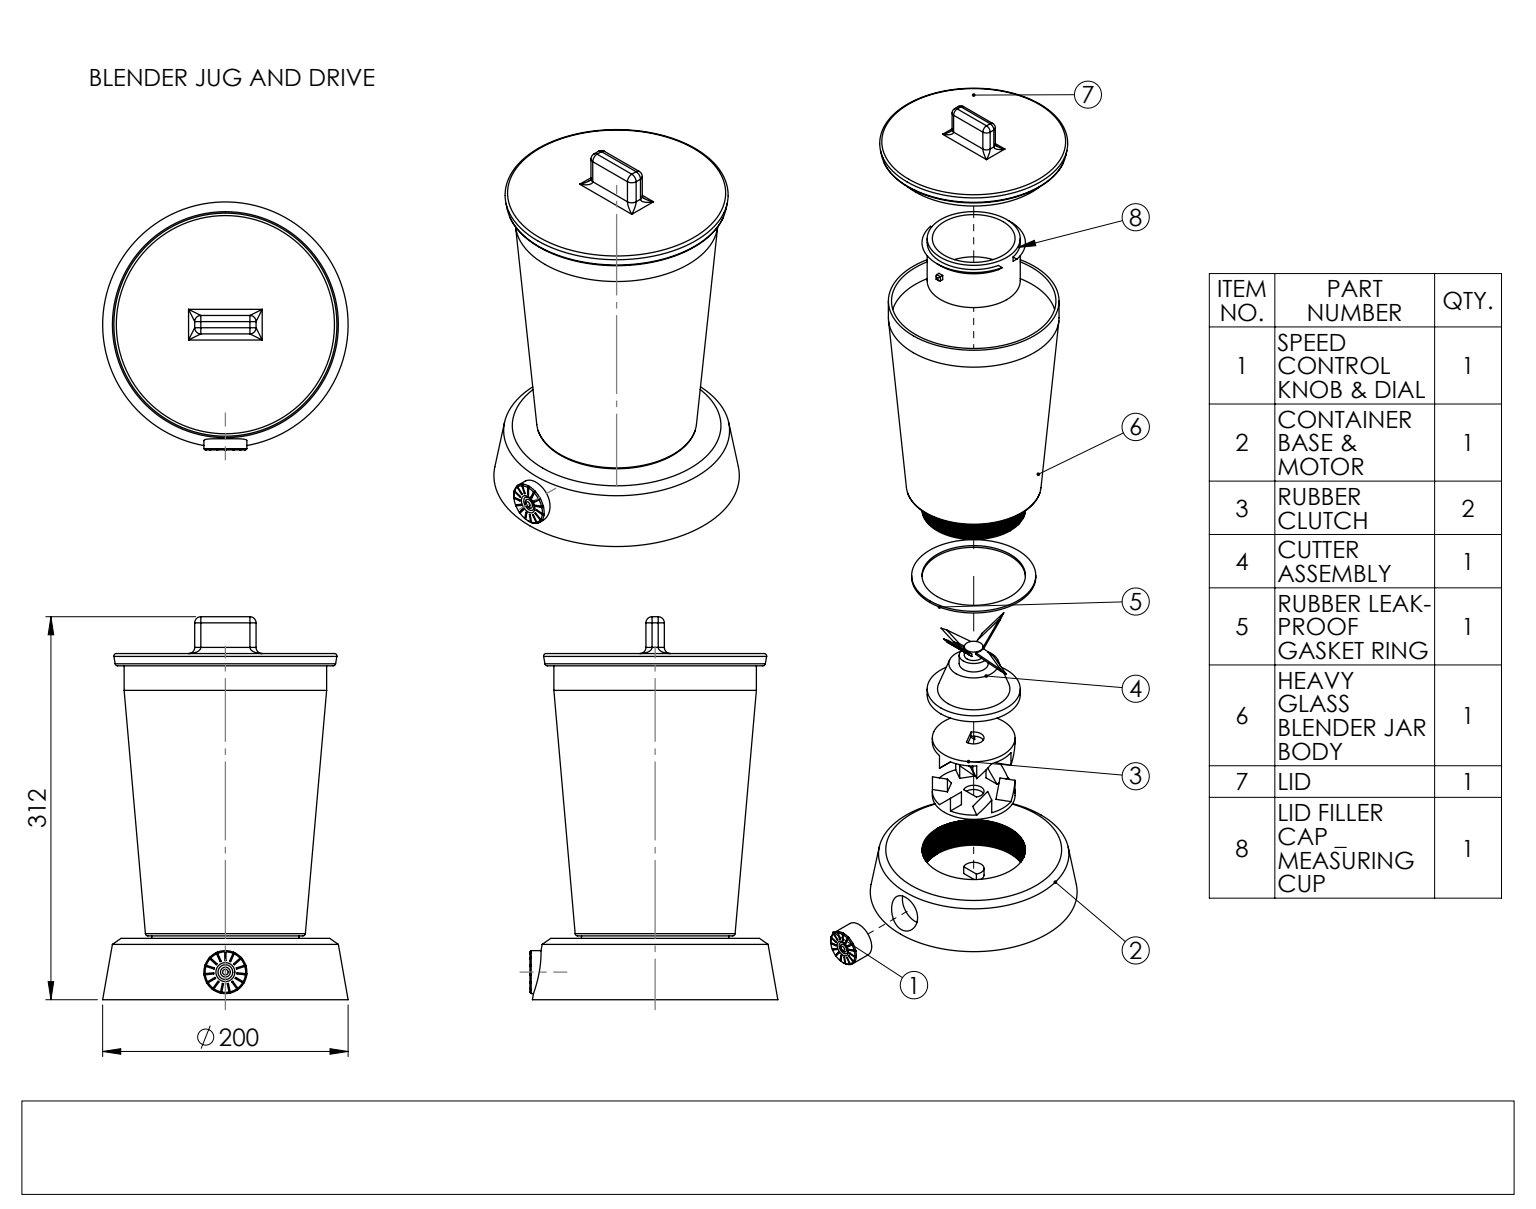
ISO-10303-21;
HEADER;
FILE_DESCRIPTION (('STEP AP214'),
    '1' );
FILE_NAME ('BR-819',
    '2026-10-09T15:02:13',
    ( '' ),
    ( '' ),
    'SwSTEP 2.0',
    'SolidWorks 2026',
    '' );
FILE_SCHEMA (( 'AUTOMOTIVE_DESIGN' ));
ENDSEC;

DATA;
#1 = EDGE_CURVE ( 'NONE', #9758, #2312, #3659, .T. ) ;
#2 = ORIENTED_EDGE ( 'NONE', *, *, #5817, .T. ) ;
#3 = DIRECTION ( 'NONE',  ( 0.000000000000000000, 0.000000000000000000, 1.000000000000000000 ) ) ;
#4 = CARTESIAN_POINT ( 'NONE',  ( -40.34137639590981905, 29.65937500034139518, -29.30972558990011478 ) ) ;
#5 = ORIENTED_EDGE ( 'NONE', *, *, #13422, .T. ) ;
#6 = DIRECTION ( 'NONE',  ( 0.000000000000000000, 0.000000000000000000, 1.000000000000000000 ) ) ;
#7 = CARTESIAN_POINT ( 'NONE',  ( 9.881733417930924190, 8.048309972292271297, 101.0000000000000000 ) ) ;
#8 = CARTESIAN_POINT ( 'NONE',  ( 47.50025713571348263, 25.00000000000000000, -15.17274647889483496 ) ) ;
#9 = CARTESIAN_POINT ( 'NONE',  ( 49.86468353124999453, 35.02187500034139589, -16.20201782572376104 ) ) ;
#10 = EDGE_CURVE ( 'NONE', #4476, #13481, #11027, .T. ) ;
#11 = LINE ( 'NONE', #4013, #8670 ) ;
#12 = CARTESIAN_POINT ( 'NONE',  ( -15.40903463028480580, 24.25937500034139660, 47.42413220539094709 ) ) ;
#13 = LINE ( 'NONE', #15220, #1773 ) ;
#14 = CARTESIAN_POINT ( 'NONE',  ( -49.86468353124999453, 37.82187500034139305, -16.20201782572375393 ) ) ;
#15 = DIRECTION ( 'NONE',  ( 0.000000000000000000, 0.9961946980917455452, 0.08715574274765836016 ) ) ;
#16 = CARTESIAN_POINT ( 'NONE',  ( -3.219174618344376363E-15, 29.49999999999999645, -52.57311121191334990 ) ) ;
#17 = CARTESIAN_POINT ( 'NONE',  ( 30.81806926056962936, 37.15937500034139873, -42.41743335407647209 ) ) ;
#18 = CARTESIAN_POINT ( 'NONE',  ( 15.40903463028481113, 31.32187500034139305, -47.42413220539094709 ) ) ;
#19 = CARTESIAN_POINT ( 'NONE',  ( 40.45084971874737079, 45.20000000000000284, -29.38926261462366440 ) ) ;
#20 = EDGE_LOOP ( 'NONE', ( #5130, #12789, #9074, #13639 ) ) ;
#21 = EDGE_LOOP ( 'NONE', ( #2044, #4544 ) ) ;
#22 = CARTESIAN_POINT ( 'NONE',  ( -30.81806926056962226, 34.15937500034139163, 42.41743335407647209 ) ) ;
#23 = ORIENTED_EDGE ( 'NONE', *, *, #4819, .F. ) ;
#24 = ORIENTED_EDGE ( 'NONE', *, *, #13474, .T. ) ;
#25 = CARTESIAN_POINT ( 'NONE',  ( 21.01167039530690062, 284.7842439685853719, -8.005835197659997959 ) ) ;
#26 = CARTESIAN_POINT ( 'NONE',  ( -40.45084971874737079, 19.98125000068279888, 29.38926261462367151 ) ) ;
#27 = CARTESIAN_POINT ( 'NONE',  ( -30.90169943749473447, 34.29999999999999005, 42.53254041760200721 ) ) ;
#28 = CARTESIAN_POINT ( 'NONE',  ( 15.40903463028481113, 21.32187500034139660, -47.42413220539094709 ) ) ;
#29 = EDGE_CURVE ( 'NONE', #8003, #7684, #9198, .T. ) ;
#30 = LINE ( 'NONE', #10110, #8655 ) ;
#31 = CARTESIAN_POINT ( 'NONE',  ( 15.40903463028482356, 44.52187500034139589, 47.42413220539093999 ) ) ;
#32 = CARTESIAN_POINT ( 'NONE',  ( -49.93234176562499727, 49.82031250051209526, 0.000000000000000000 ) ) ;
#33 = CARTESIAN_POINT ( 'NONE',  ( -40.45084971874737789, 45.79999999999999716, -29.38926261462365730 ) ) ;
#34 = CARTESIAN_POINT ( 'NONE',  ( -15.45084971874736368, 26.18125000068280173, 47.55282581475768211 ) ) ;
#35 = DIRECTION ( 'NONE',  ( -0.8660254037844327124, 0.000000000000000000, 0.5000000000000102141 ) ) ;
#36 = CARTESIAN_POINT ( 'NONE',  ( -3.210462471511496205E-15, 31.42187500034139447, -52.43083105670540789 ) ) ;
#37 = CARTESIAN_POINT ( 'NONE',  ( -24.78626291527390890, 25.00000000000000355, 5.650101528493965297 ) ) ;
#38 = CARTESIAN_POINT ( 'NONE',  ( -0.5000000000000000000, 247.0000000000000284, -49.99999999999999289 ) ) ;
#39 = ORIENTED_EDGE ( 'NONE', *, *, #2245, .T. ) ;
#40 = VERTEX_POINT ( 'NONE', #9811 ) ;
#41 = EDGE_CURVE ( 'NONE', #13641, #5789, #12730, .T. ) ;
#42 = CARTESIAN_POINT ( 'NONE',  ( 30.27664397204074476, 25.00000000000000355, 26.14048258526015189 ) ) ;
#43 = FACE_OUTER_BOUND ( 'NONE', #155, .T. ) ;
#44 = DIRECTION ( 'NONE',  ( 0.000000000000000000, -0.000000000000000000, 1.000000000000000000 ) ) ;
#45 = CARTESIAN_POINT ( 'NONE',  ( -2.547328955960238000E-13, 24.28125000068279604, 49.99999999999999289 ) ) ;
#46 = CARTESIAN_POINT ( 'NONE',  ( -3.210462471511496205E-15, 33.35937500034140157, -52.43083105670540789 ) ) ;
#47 =( NAMED_UNIT ( * ) SI_UNIT ( $, .STERADIAN. ) SOLID_ANGLE_UNIT ( ) );
#48 = CARTESIAN_POINT ( 'NONE',  ( 49.86468353125001585, 46.82187500034139305, 16.20201782572375038 ) ) ;
#49 =( NAMED_UNIT ( * ) PLANE_ANGLE_UNIT ( ) SI_UNIT ( $, .RADIAN. ) );
#50 = LINE ( 'NONE', #11218, #7284 ) ;
#51 = CARTESIAN_POINT ( 'NONE',  ( -30.00000000000000711, 282.0000000000000000, 0.000000000000000000 ) ) ;
#52 = ORIENTED_EDGE ( 'NONE', *, *, #15437, .T. ) ;
#53 = AXIS2_PLACEMENT_3D ( 'NONE', #15949, #12213, #9481 ) ;
#54 = CARTESIAN_POINT ( 'NONE',  ( -15.40903463028481646, 25.45937500034139589, -47.42413220539093999 ) ) ;
#55 = ORIENTED_EDGE ( 'NONE', *, *, #4586, .T. ) ;
#56 = CARTESIAN_POINT ( 'NONE',  ( -40.45084971874737789, 25.80000000000000071, -29.38926261462365730 ) ) ;
#57 = ORIENTED_EDGE ( 'NONE', *, *, #15029, .T. ) ;
#58 = VERTEX_POINT ( 'NONE', #12787 ) ;
#59 = FACE_OUTER_BOUND ( 'NONE', #13989, .T. ) ;
#60 = CARTESIAN_POINT ( 'NONE',  ( 48.98979485566356118, 261.9999999999999432, -10.00000000000000178 ) ) ;
#61 = CARTESIAN_POINT ( 'NONE',  ( -1.240322475938754499E-13, 36.28125000068280315, 50.00000000000000000 ) ) ;
#62 = CARTESIAN_POINT ( 'NONE',  ( -16.78599477205477797, 21.23847499609123801, 101.6666710451724214 ) ) ;
#63 = CARTESIAN_POINT ( 'NONE',  ( 2.600676159226420495E-13, 33.28125000068279604, -49.99999999999999289 ) ) ;
#64 = CARTESIAN_POINT ( 'NONE',  ( 0.000000000000000000, 22.50000000000000000, 101.0000000000000000 ) ) ;
#65 = DIRECTION ( 'NONE',  ( 0.9945218953682730678, 0.1045284632676572317, 0.000000000000000000 ) ) ;
#66 = CARTESIAN_POINT ( 'NONE',  ( 9.262651381018932677E-15, 92.00000000000001421, -9.080892972013931086 ) ) ;
#67 = VECTOR ( 'NONE', #6603, 999.9999999999998863 ) ;
#68 = SURFACE_SIDE_STYLE ('',( #9066 ) ) ;
#69 = CARTESIAN_POINT ( 'NONE',  ( -7.919222016226809657, 49.55125428154685352, -49.99999999999999289 ) ) ;
#70 = CARTESIAN_POINT ( 'NONE',  ( -49.99999999999999289, 39.88125000068279746, 16.24598481164533226 ) ) ;
#71 = ADVANCED_FACE ( 'NONE', ( #2644 ), #15361, .T. ) ;
#72 = CARTESIAN_POINT ( 'NONE',  ( -49.99999999999999289, 23.90000000000000213, -16.24598481164531449 ) ) ;
#73 = EDGE_CURVE ( 'NONE', #16417, #15936, #15440, .T. ) ;
#74 = CARTESIAN_POINT ( 'NONE',  ( 1.041190247313760726E-14, 50.00000000000000000, 85.01963570546854498 ) ) ;
#75 = VERTEX_POINT ( 'NONE', #14029 ) ;
#76 = CARTESIAN_POINT ( 'NONE',  ( 49.86468353124999453, 44.95937500034139589, -16.20201782572376459 ) ) ;
#77 = ORIENTED_EDGE ( 'NONE', *, *, #283, .F. ) ;
#78 = VECTOR ( 'NONE', #10957, 1000.000000000000000 ) ;
#79 = DIRECTION ( 'NONE',  ( -0.000000000000000000, -1.000000000000000000, -0.000000000000000000 ) ) ;
#80 = CARTESIAN_POINT ( 'NONE',  ( -49.86468353124999453, 25.95937500034139944, 16.20201782572377525 ) ) ;
#81 = VERTEX_POINT ( 'NONE', #16451 ) ;
#82 = CARTESIAN_POINT ( 'NONE',  ( 0.000000000000000000, 22.50000000000000000, 80.00000000000000000 ) ) ;
#84 = ADVANCED_FACE ( 'NONE', ( #9052 ), #9129, .T. ) ;
#83 = CARTESIAN_POINT ( 'NONE',  ( -17.47289750917834539, 23.62647710751876318, 94.22769020256006911 ) ) ;
#85 = CARTESIAN_POINT ( 'NONE',  ( 47.13255506291616115, 25.00000000000000711, -16.27994764699579022 ) ) ;
#86 = CARTESIAN_POINT ( 'NONE',  ( -15.40903463028480580, 34.32187500034139305, 47.42413220539094709 ) ) ;
#87 =( BOUNDED_CURVE ( )  B_SPLINE_CURVE ( 2, ( #12702, #8875, #13934, #16199, #7548, #15262, #4829, #3730, #6314, #2555, #11379, #10211, #16445 ),
 .UNSPECIFIED., .F., .F. ) 
 B_SPLINE_CURVE_WITH_KNOTS ( ( 3, 2, 2, 2, 2, 2, 3 ),
 ( 0.3166666666666667074, 0.3200000000000000067, 0.3266666666666666607, 0.3333333333333333148, 0.3400000000000000244, 0.3466666666666666785, 0.3500000000000000333 ),
 .UNSPECIFIED. ) 
 CURVE ( )  GEOMETRIC_REPRESENTATION_ITEM ( )  RATIONAL_B_SPLINE_CURVE ( ( 0.9755282581475768211, 0.9755282581475770431, 1.000000000000000000, 0.9510565162951535312, 1.000000000000000000, 0.9510565162951535312, 1.000000000000000000, 0.9510565162951535312, 1.000000000000000000, 0.9510565162951535312, 1.000000000000000000, 0.9755282581475765991, 0.9755282581475768211 ) ) 
 REPRESENTATION_ITEM ( '' )  );
#88 = CARTESIAN_POINT ( 'NONE',  ( 25.00000000000000000, 284.0710678118655323, -2.499999999999998224 ) ) ;
#89 = CARTESIAN_POINT ( 'NONE',  ( 49.86468353125000164, 20.85937500034139802, -6.106662507704105588E-15 ) ) ;
#90 = DIRECTION ( 'NONE',  ( -2.126576849575776229E-17, -0.9848077530122080203, -0.1736481776669307198 ) ) ;
#91 = CARTESIAN_POINT ( 'NONE',  ( 30.81806926056962936, 27.22187500034139518, -42.41743335407646498 ) ) ;
#92 = LINE ( 'NONE', #7754, #12118 ) ;
#93 = AXIS2_PLACEMENT_3D ( 'NONE', #810, #7225, #14526 ) ;
#94 = CARTESIAN_POINT ( 'NONE',  ( 30.90169943749474157, 29.30000000000000071, -42.53254041760200721 ) ) ;
#95 = CARTESIAN_POINT ( 'NONE',  ( -49.86468353124999453, 35.95937500034139589, 16.20201782572377525 ) ) ;
#96 = CARTESIAN_POINT ( 'NONE',  ( 30.81806926056964002, 30.62187500034139020, 42.41743335407647209 ) ) ;
#97 = CARTESIAN_POINT ( 'NONE',  ( 49.99999999999999289, 41.10000000000000853, -16.24598481164532160 ) ) ;
#98 = ORIENTED_EDGE ( 'NONE', *, *, #10995, .T. ) ;
#99 = EDGE_CURVE ( 'NONE', #10795, #16436, #8019, .T. ) ;
#100 = UNCERTAINTY_MEASURE_WITH_UNIT (LENGTH_MEASURE( 1.000000000000000082E-05 ), #13795, 'distance_accuracy_value', 'NONE');
#101 = CARTESIAN_POINT ( 'NONE',  ( -40.34137639590981905, 35.65937500034139873, -29.30972558990011478 ) ) ;
#102 = VERTEX_POINT ( 'NONE', #7719 ) ;
#103 = CARTESIAN_POINT ( 'NONE',  ( 28.07127062163609210, 282.3184422169448453, -10.57127062163368691 ) ) ;
#104 = CARTESIAN_POINT ( 'NONE',  ( -30.81806926056963292, 47.55937500034139731, -42.41743335407647209 ) ) ;
#105 = CARTESIAN_POINT ( 'NONE',  ( 0.000000000000000000, 261.9999999999999432, 49.99999999999999289 ) ) ;
#106 = CARTESIAN_POINT ( 'NONE',  ( -49.86468353124999453, 23.82187500034139305, -16.20201782572375393 ) ) ;
#107 = CARTESIAN_POINT ( 'NONE',  ( 0.000000000000000000, 22.50000000000000000, 102.0000000000000142 ) ) ;
#108 = CARTESIAN_POINT ( 'NONE',  ( -40.34137639590981195, 44.12187500034139731, 29.30972558990012189 ) ) ;
#109 = CARTESIAN_POINT ( 'NONE',  ( -15.40903463028481646, 39.45937500034139589, -47.42413220539093999 ) ) ;
#110 = LINE ( 'NONE', #6455, #15051 ) ;
#111 = CARTESIAN_POINT ( 'NONE',  ( 40.45084971874737789, 44.79999999999999716, 29.38926261462365375 ) ) ;
#112 = EDGE_CURVE ( 'NONE', #12675, #13582, #5642, .T. ) ;
#113 = CARTESIAN_POINT ( 'NONE',  ( -49.99999999999999289, 25.68125000068279462, -16.24598481164531449 ) ) ;
#114 = CARTESIAN_POINT ( 'NONE',  ( 15.22000719008740077, 31.21383541804545914, 93.26445288283514401 ) ) ;
#115 = CIRCLE ( 'NONE', #5192, 45.00000000000000000 ) ;
#116 = CARTESIAN_POINT ( 'NONE',  ( 15.40903463028482356, 32.52187500034139589, 47.42413220539093999 ) ) ;
#117 = CARTESIAN_POINT ( 'NONE',  ( -3.505380114644273348, 97.73782665365220623, 8.566253778398339236 ) ) ;
#118 = ORIENTED_EDGE ( 'NONE', *, *, #603, .F. ) ;
#119 = ORIENTED_EDGE ( 'NONE', *, *, #8529, .T. ) ;
#120 = CARTESIAN_POINT ( 'NONE',  ( -30.90169943749473447, 32.30000000000000426, 42.53254041760200721 ) ) ;
#121 = AXIS2_PLACEMENT_3D ( 'NONE', #2630, #13768, #2460 ) ;
#122 = CARTESIAN_POINT ( 'NONE',  ( -40.45084971874737789, 23.80000000000000071, -29.38926261462365730 ) ) ;
#123 = CARTESIAN_POINT ( 'NONE',  ( -49.86468353124999453, 48.02187500034139589, 16.20201782572377169 ) ) ;
#124 = CARTESIAN_POINT ( 'NONE',  ( 9.631387414534489405E-15, 34.35937500034139447, 52.43083105670540789 ) ) ;
#125 = EDGE_CURVE ( 'NONE', #10026, #5291, #8135, .T. ) ;
#126 = FACE_OUTER_BOUND ( 'NONE', #347, .T. ) ;
#127 = EDGE_CURVE ( 'NONE', #6081, #8153, #2564, .T. ) ;
#128 = CARTESIAN_POINT ( 'NONE',  ( 49.86468353125001585, 44.82187500034139305, 16.20201782572375038 ) ) ;
#129 =( NAMED_UNIT ( * ) SI_UNIT ( $, .STERADIAN. ) SOLID_ANGLE_UNIT ( ) );
#130 = DIRECTION ( 'NONE',  ( 0.000000000000000000, 0.000000000000000000, -1.000000000000000000 ) ) ;
#131 = DIRECTION ( 'NONE',  ( 0.000000000000000000, 0.000000000000000000, -1.000000000000000000 ) ) ;
#132 = DIRECTION ( 'NONE',  ( 0.000000000000000000, 0.000000000000000000, 1.000000000000000000 ) ) ;
#133 = ORIENTED_EDGE ( 'NONE', *, *, #7031, .F. ) ;
#134 = AXIS2_PLACEMENT_3D ( 'NONE', #8238, #4509, #8316 ) ;
#135 = CARTESIAN_POINT ( 'NONE',  ( -15.40903463028481646, 47.52187500034139589, -47.42413220539093999 ) ) ;
#136 = ORIENTED_EDGE ( 'NONE', *, *, #8247, .T. ) ;
#137 = DIRECTION ( 'NONE',  ( 0.5000000000000039968, -0.8660254037844363761, 0.000000000000000000 ) ) ;
#138 = ORIENTED_EDGE ( 'NONE', *, *, #3634, .T. ) ;
#139 = ORIENTED_EDGE ( 'NONE', *, *, #8040, .T. ) ;
#140 = AXIS2_PLACEMENT_3D ( 'NONE', #851, #930, #4703 ) ;
#141 = DIRECTION ( 'NONE',  ( 0.000000000000000000, 0.000000000000000000, -1.000000000000000000 ) ) ;
#142 = ADVANCED_FACE ( 'NONE', ( #11706 ), #1477, .T. ) ;
#143 = CARTESIAN_POINT ( 'NONE',  ( 5.000000000000000000, 90.58578643762692195, -1.414213562373097588 ) ) ;
#144 = PLANE ( 'NONE',  #9294 ) ;
#145 = DIRECTION ( 'NONE',  ( 0.000000000000000000, 1.000000000000000000, 0.000000000000000000 ) ) ;
#146 = VECTOR ( 'NONE', #14798, 1000.000000000000000 ) ;
#147 = EDGE_CURVE ( 'NONE', #1228, #14186, #15189, .T. ) ;
#148 = PLANE ( 'NONE',  #13952 ) ;
#149 = LINE ( 'NONE', #6489, #8395 ) ;
#150 = AXIS2_PLACEMENT_3D ( 'NONE', #12776, #1296, #13929 ) ;
#151 = CIRCLE ( 'NONE', #2279, 50.00000000000000000 ) ;
#152 = CARTESIAN_POINT ( 'NONE',  ( -30.90169943749473447, 32.08125000068280031, 42.53254041760200721 ) ) ;
#153 = FACE_OUTER_BOUND ( 'NONE', #12318, .T. ) ;
#154 = SURFACE_SIDE_STYLE ('',( #7731 ) ) ;
#155 = EDGE_LOOP ( 'NONE', ( #7318, #4198, #8287 ) ) ;
#156 = CARTESIAN_POINT ( 'NONE',  ( -30.90169943749474513, 49.70000000000000284, -42.53254041760200721 ) ) ;
#157 = CARTESIAN_POINT ( 'NONE',  ( -40.45084971874737079, 41.98125000068279888, 29.38926261462367151 ) ) ;
#158 = DIRECTION ( 'NONE',  ( -0.000000000000000000, 1.000000000000000000, -0.000000000000000000 ) ) ;
#159 = EDGE_CURVE ( 'NONE', #15854, #13562, #284, .T. ) ;
#160 = CARTESIAN_POINT ( 'NONE',  ( 15.45084971874737789, 20.60000000000000142, 47.55282581475767500 ) ) ;
#161 = PRESENTATION_STYLE_ASSIGNMENT (( #5178 ) ) ;
#162 = ORIENTED_EDGE ( 'NONE', *, *, #15184, .T. ) ;
#163 = CARTESIAN_POINT ( 'NONE',  ( -49.86468353124999453, 37.95937500034140299, 16.20201782572377525 ) ) ;
#164 = CIRCLE ( 'NONE', #9467, 45.00000000000000000 ) ;
#165 = ORIENTED_EDGE ( 'NONE', *, *, #12600, .T. ) ;
#166 = VECTOR ( 'NONE', #9002, 1000.000000000000000 ) ;
#167 = AXIS2_PLACEMENT_3D ( 'NONE', #3146, #15868, #1731 ) ;
#168 = AXIS2_PLACEMENT_3D ( 'NONE', #2091, #15059, #8742 ) ;
#169 = CARTESIAN_POINT ( 'NONE',  ( 49.99999999999999289, 42.88125000068279036, -16.24598481164532160 ) ) ;
#170 = CARTESIAN_POINT ( 'NONE',  ( -1.240322475938754499E-13, 38.28125000068280315, 50.00000000000000000 ) ) ;
#171 = CARTESIAN_POINT ( 'NONE',  ( -40.34137639590981905, 31.65937500034139873, -29.30972558990011478 ) ) ;
#172 = VERTEX_POINT ( 'NONE', #11782 ) ;
#173 = CARTESIAN_POINT ( 'NONE',  ( 2.600676159226421000E-13, 31.49999999999999289, -49.99999999999999289 ) ) ;
#174 = CARTESIAN_POINT ( 'NONE',  ( 14.53285685708578256, 14.68680145065703080, 102.0000000000000142 ) ) ;
#175 = CARTESIAN_POINT ( 'NONE',  ( 46.62157290631164130, 24.99999999999999289, -17.69020581816995730 ) ) ;
#176 = CARTESIAN_POINT ( 'NONE',  ( -40.34137639590981195, 32.12187500034140442, 29.30972558990012189 ) ) ;
#177 = CARTESIAN_POINT ( 'NONE',  ( 30.90169943749475223, 46.48125000068280599, 42.53254041760199300 ) ) ;
#178 = CIRCLE ( 'NONE', #9484, 17.50000000000000000 ) ;
#179 = CARTESIAN_POINT ( 'NONE',  ( 15.40903463028482356, 24.45937500034139589, 47.42413220539093999 ) ) ;
#180 = CARTESIAN_POINT ( 'NONE',  ( -9.189545401991425777, 24.96013318841439599, 102.0000000000000142 ) ) ;
#181 = CARTESIAN_POINT ( 'NONE',  ( 49.86468353125000164, 28.92187500034139802, -6.106662507704105588E-15 ) ) ;
#182 = CARTESIAN_POINT ( 'NONE',  ( 9.227956911499398113E-15, 102.0000000000000142, -9.080892972013931086 ) ) ;
#183 = CARTESIAN_POINT ( 'NONE',  ( 15.45084971874737789, 28.60000000000000142, 47.55282581475767500 ) ) ;
#184 = CARTESIAN_POINT ( 'NONE',  ( 40.34137639590981905, 32.65937500034139873, 29.30972558990010768 ) ) ;
#185 = CARTESIAN_POINT ( 'NONE',  ( 9.631387414534489405E-15, 32.42187500034139447, 52.43083105670540789 ) ) ;
#186 = ORIENTED_EDGE ( 'NONE', *, *, #13105, .F. ) ;
#187 = CARTESIAN_POINT ( 'NONE',  ( 40.34137639590981195, 33.05937500034139731, -29.30972558990011834 ) ) ;
#188 = ORIENTED_EDGE ( 'NONE', *, *, #204, .F. ) ;
#189 = ORIENTED_EDGE ( 'NONE', *, *, #1369, .F. ) ;
#190 = CARTESIAN_POINT ( 'NONE',  ( 24.98849325795415766, 282.6608420050619088, -9.994246628976295455 ) ) ;
#192 =( BOUNDED_CURVE ( )  B_SPLINE_CURVE ( 2, ( #6981, #12037, #4493, #8380, #732, #13454, #3955, #10196, #11517, #15248, #2623, #11683, #15338 ),
 .UNSPECIFIED., .F., .T. ) 
 B_SPLINE_CURVE_WITH_KNOTS ( ( 3, 2, 2, 2, 2, 2, 3 ),
 ( 0.4500000000000000111, 0.4533333333333333104, 0.4600000000000000200, 0.4666666666666666741, 0.4733333333333333282, 0.4799999999999999822, 0.4833333333333333370 ),
 .UNSPECIFIED. ) 
 CURVE ( )  GEOMETRIC_REPRESENTATION_ITEM ( )  RATIONAL_B_SPLINE_CURVE ( ( 0.9755282581475768211, 0.9755282581475770431, 1.000000000000000000, 0.9510565162951535312, 1.000000000000000000, 0.9510565162951535312, 1.000000000000000000, 0.9510565162951535312, 1.000000000000000000, 0.9510565162951535312, 1.000000000000000000, 0.9755282581475768211, 0.9755282581475768211 ) ) 
 REPRESENTATION_ITEM ( '' )  );
#191 = CARTESIAN_POINT ( 'NONE',  ( -30.90169943749473802, 20.08125000068279320, 42.53254041760200721 ) ) ;
#193 = CARTESIAN_POINT ( 'NONE',  ( 0.000000000000000000, 22.50000000000000000, 102.0000000000000142 ) ) ;
#194 = CARTESIAN_POINT ( 'NONE',  ( 30.81806926056964002, 26.62187500034139731, 42.41743335407647209 ) ) ;
#195 = DIRECTION ( 'NONE',  ( -0.4067366430758010409, 0.9135454576426005335, 0.000000000000000000 ) ) ;
#196 = CARTESIAN_POINT ( 'NONE',  ( 15.40903463028481113, 37.32187500034140015, -47.42413220539094709 ) ) ;
#197 = CARTESIAN_POINT ( 'NONE',  ( 15.40903463028482356, 44.45937500034139589, 47.42413220539093999 ) ) ;
#198 = DIRECTION ( 'NONE',  ( 0.8660254037844513642, 0.4999999999999780731, 0.000000000000000000 ) ) ;
#199 = EDGE_CURVE ( 'NONE', #14735, #10689, #4239, .T. ) ;
#200 = CARTESIAN_POINT ( 'NONE',  ( 30.90169943749474157, 49.29999999999999716, -42.53254041760200721 ) ) ;
#201 = CARTESIAN_POINT ( 'NONE',  ( -15.45084971874736368, 20.18125000068279817, 47.55282581475768211 ) ) ;
#202 = CARTESIAN_POINT ( 'NONE',  ( 5.000000000000000000, 96.75198296766784267, -7.580410092414001433 ) ) ;
#203 = CARTESIAN_POINT ( 'NONE',  ( -49.86468353124999453, 28.02187500034139234, 16.20201782572377525 ) ) ;
#204 = EDGE_CURVE ( 'NONE', #5010, #3842, #426, .T. ) ;
#205 = EDGE_CURVE ( 'NONE', #75, #14665, #7073, .T. ) ;
#206 = EDGE_LOOP ( 'NONE', ( #10234, #136 ) ) ;
#207 = CARTESIAN_POINT ( 'NONE',  ( 50.00000000000000000, 36.78125000068280315, -6.123233995736766085E-15 ) ) ;
#208 = AXIS2_PLACEMENT_3D ( 'NONE', #5247, #15355, #10131 ) ;
#209 = ORIENTED_EDGE ( 'NONE', *, *, #12461, .T. ) ;
#210 = EDGE_CURVE ( 'NONE', #11778, #8192, #3075, .T. ) ;
#211 = CARTESIAN_POINT ( 'NONE',  ( 49.99999999999999289, 48.88125000068280457, -16.24598481164532160 ) ) ;
#212 = CARTESIAN_POINT ( 'NONE',  ( 0.000000000000000000, 22.50000000000000000, 101.0000000000000000 ) ) ;
#213 = EDGE_CURVE ( 'NONE', #982, #10751, #1081, .T. ) ;
#214 = DIRECTION ( 'NONE',  ( 6.938893903907231459E-18, -1.000000000000000000, -5.551115123125782702E-17 ) ) ;
#215 = CARTESIAN_POINT ( 'NONE',  ( 49.86468353124999453, 45.02187500034138878, -16.20201782572376104 ) ) ;
#216 = CARTESIAN_POINT ( 'NONE',  ( 49.86468353125000164, 30.85937500034139802, -6.106662507704105588E-15 ) ) ;
#217 = CYLINDRICAL_SURFACE ( 'NONE', #11583, 50.00000000000000000 ) ;
#218 = PLANE ( 'NONE',  #7160 ) ;
#219 = CARTESIAN_POINT ( 'NONE',  ( -49.86468353124999453, 47.82187500034140015, -16.20201782572375393 ) ) ;
#220 =( NAMED_UNIT ( * ) SI_UNIT ( $, .STERADIAN. ) SOLID_ANGLE_UNIT ( ) );
#221 = CARTESIAN_POINT ( 'NONE',  ( 50.00000000000000000, 34.78125000068280315, -6.123233995736766085E-15 ) ) ;
#222 = CARTESIAN_POINT ( 'NONE',  ( -40.34137639590981905, 47.72187500034139873, -29.30972558990011478 ) ) ;
#223 = DIRECTION ( 'NONE',  ( 0.000000000000000000, -1.000000000000000000, 0.000000000000000000 ) ) ;
#224 = ORIENTED_EDGE ( 'NONE', *, *, #8585, .T. ) ;
#225 = CARTESIAN_POINT ( 'NONE',  ( -49.86468353125000164, 45.92187500034139447, 0.000000000000000000 ) ) ;
#226 = ORIENTED_EDGE ( 'NONE', *, *, #2314, .T. ) ;
#227 = DIRECTION ( 'NONE',  ( 0.000000000000000000, 0.000000000000000000, -1.000000000000000000 ) ) ;
#228 = EDGE_LOOP ( 'NONE', ( #7013, #1311, #10553, #6194 ) ) ;
#229 = ORIENTED_EDGE ( 'NONE', *, *, #5927, .T. ) ;
#230 = DIRECTION ( 'NONE',  ( 0.000000000000000000, 0.000000000000000000, 1.000000000000000000 ) ) ;
#231 = CARTESIAN_POINT ( 'NONE',  ( -49.72257916183962578, 96.64601816452537264, -5.000000000000008882 ) ) ;
#232 = CARTESIAN_POINT ( 'NONE',  ( -40.45084971874737789, 21.80000000000000071, -29.38926261462365730 ) ) ;
#233 = AXIS2_PLACEMENT_3D ( 'NONE', #3422, #4672, #16139 ) ;
#234 = CARTESIAN_POINT ( 'NONE',  ( -49.86468353125000164, 49.85937500034139447, 0.000000000000000000 ) ) ;
#235 = CARTESIAN_POINT ( 'NONE',  ( 9.332040320058006538E-15, 82.00000000000001421, -14.08089297201393286 ) ) ;
#236 = PLANE ( 'NONE',  #13502 ) ;
#237 = CARTESIAN_POINT ( 'NONE',  ( -30.81806926056962226, 26.22187500034139518, 42.41743335407647919 ) ) ;
#238 = DIRECTION ( 'NONE',  ( -0.9510565162951503115, -0.3090169943749574988, 0.000000000000000000 ) ) ;
#239 = CARTESIAN_POINT ( 'NONE',  ( -50.00000000000000000, 37.78125000068280315, 0.000000000000000000 ) ) ;
#240 = DIRECTION ( 'NONE',  ( 0.000000000000000000, 1.000000000000000000, 0.000000000000000000 ) ) ;
#241 = CARTESIAN_POINT ( 'NONE',  ( -50.00000000000000000, 20.00000000000000000, 0.000000000000000000 ) ) ;
#242 = LINE ( 'NONE', #9147, #15465 ) ;
#243 = VERTEX_POINT ( 'NONE', #6253 ) ;
#244 = CARTESIAN_POINT ( 'NONE',  ( -3.210462471511496205E-15, 39.35937500034138736, -52.43083105670540789 ) ) ;
#245 = VECTOR ( 'NONE', #10822, 1000.000000000000000 ) ;
#246 = ORIENTED_EDGE ( 'NONE', *, *, #11483, .F. ) ;
#247 = CARTESIAN_POINT ( 'NONE',  ( 49.99999999999999289, 48.88125000068279746, -16.24598481164532160 ) ) ;
#248 = DIRECTION ( 'NONE',  ( 0.000000000000000000, 0.000000000000000000, 1.000000000000000000 ) ) ;
#249 = CARTESIAN_POINT ( 'NONE',  ( -49.86468353124999453, 31.75937500034140015, -16.20201782572375393 ) ) ;
#250 = ORIENTED_EDGE ( 'NONE', *, *, #6640, .T. ) ;
#251 = EDGE_CURVE ( 'NONE', #6737, #5002, #13879, .T. ) ;
#252 = CARTESIAN_POINT ( 'NONE',  ( 50.00000000000000711, 26.89999999999999858, 16.24598481164530739 ) ) ;
#253 = CARTESIAN_POINT ( 'NONE',  ( -13.94098003074309844, 33.14011566961073640, 93.12075586326798771 ) ) ;
#254 = CARTESIAN_POINT ( 'NONE',  ( -15.39925740754308059, 14.18658485962419569, 101.0000000000000000 ) ) ;
#255 = CARTESIAN_POINT ( 'NONE',  ( 30.81806926056962936, 35.22187500034138452, -42.41743335407646498 ) ) ;
#256 = DIRECTION ( 'NONE',  ( 1.000000000000000000, -0.000000000000000000, 0.000000000000000000 ) ) ;
#257 = CARTESIAN_POINT ( 'NONE',  ( 40.34137639590981195, 21.05937500034139376, -29.30972558990011834 ) ) ;
#258 = CARTESIAN_POINT ( 'NONE',  ( 6.123233995736766085E-15, 20.00000000000000355, -50.00000000000000000 ) ) ;
#259 = CARTESIAN_POINT ( 'NONE',  ( 15.40903463028481113, 27.32187500034139660, -47.42413220539094709 ) ) ;
#260 = CARTESIAN_POINT ( 'NONE',  ( 0.000000000000000000, 257.0000000000001137, 0.000000000000000000 ) ) ;
#261 = CARTESIAN_POINT ( 'NONE',  ( 50.00000000000000711, 30.89999999999999503, 16.24598481164530739 ) ) ;
#262 = CARTESIAN_POINT ( 'NONE',  ( 30.81806926056962936, 29.15937500034139518, -42.41743335407647209 ) ) ;
#263 = CARTESIAN_POINT ( 'NONE',  ( -15.40903463028481646, 27.52187500034139944, -47.42413220539093999 ) ) ;
#264 = ORIENTED_EDGE ( 'NONE', *, *, #127, .F. ) ;
#265 = UNCERTAINTY_MEASURE_WITH_UNIT (LENGTH_MEASURE( 1.000000000000000082E-05 ), #1967, 'distance_accuracy_value', 'NONE');
#266 = B_SPLINE_CURVE_WITH_KNOTS ( 'NONE', 3,
 ( #13888, #7584, #1338, #3766, #3845, #12662, #9000, #3929, #8825, #2503, #1169, #9081, #15216, #1258, #12497, #11416, #1090, #15389, #12572, #6350, #6265, #8, #6428, #1418, #6182, #14058, #2674, #11488, #85, #7748, #12816, #6510, #3692, #15064, #11567, #5111, #10245, #175, #10166, #5280, #11336, #10331, #4011, #2348, #16313, #7429, #11256, #8911, #4949, #10007, #8747, #13812, #2423, #7501, #16403, #10088, #13975, #5036, #2594, #15138, #7670 ),
 .UNSPECIFIED., .F., .F.,
 ( 4, 3, 3, 3, 3, 3, 3, 3, 3, 3, 3, 3, 3, 3, 3, 3, 3, 3, 3, 3, 4 ),
 ( 5.250942343321584884E-16, 0.0001250000981872776470, 0.0006250122739946113812, 0.001125024449802053753, 0.001625036625609322868, 0.002125048801416675251, 0.002625060977223842018, 0.003125073153031292413, 0.003625085328838458312, 0.004125097504645739571, 0.004625109680452853429, 0.005125121856260251782, 0.005625134032067363038, 0.006125146207874809963, 0.006625158383682325410, 0.007125170559489371613, 0.007625182735296599096, 0.008125194911103644432, 0.008625207086911109572, 0.009137502482430032158, 0.009649851960371033655 ),
 .UNSPECIFIED. ) ;
#267 = CARTESIAN_POINT ( 'NONE',  ( 15.40903463028481113, 39.25937500034140015, -47.42413220539094709 ) ) ;
#268 = ORIENTED_EDGE ( 'NONE', *, *, #1513, .T. ) ;
#269 = B_SPLINE_CURVE_WITH_KNOTS ( 'NONE', 3,
 ( #12649, #12562, #8736, #2338 ),
 .UNSPECIFIED., .F., .F.,
 ( 4, 4 ),
 ( 2.829004760667786001E-07, 0.001414802801989366570 ),
 .UNSPECIFIED. ) ;
#270 = CARTESIAN_POINT ( 'NONE',  ( 26.95005104082769876, 283.0244618719127629, -6.400102081653807673 ) ) ;
#271 = CARTESIAN_POINT ( 'NONE',  ( -49.86468353124999453, 47.75937500034139305, -16.20201782572375393 ) ) ;
#272 = CARTESIAN_POINT ( 'NONE',  ( -49.86468353125000164, 49.85937500034139447, 0.000000000000000000 ) ) ;
#273 = CARTESIAN_POINT ( 'NONE',  ( -15.40903463028480580, 20.32187500034139660, 47.42413220539094709 ) ) ;
#274 = CARTESIAN_POINT ( 'NONE',  ( -29.67274705320269135, 282.0000000000000000, 11.84549410641580813 ) ) ;
#275 = CARTESIAN_POINT ( 'NONE',  ( -49.86468353124999453, 38.02187500034140299, 16.20201782572377525 ) ) ;
#276 = CARTESIAN_POINT ( 'NONE',  ( -49.86468353125000164, 43.85937500034140157, 0.000000000000000000 ) ) ;
#277 = LINE ( 'NONE', #1447, #969 ) ;
#278 = CARTESIAN_POINT ( 'NONE',  ( -15.45084971874736368, 40.40000000000000568, 47.55282581475768211 ) ) ;
#279 = CARTESIAN_POINT ( 'NONE',  ( -49.86468353124999453, 49.75937500034138594, -16.20201782572375393 ) ) ;
#280 = CARTESIAN_POINT ( 'NONE',  ( 13.91912017332526830, 33.12251588586428852, 93.12580776402357685 ) ) ;
#281 = EDGE_CURVE ( 'NONE', #5931, #2031, #269, .T. ) ;
#282 = CARTESIAN_POINT ( 'NONE',  ( 15.40903463028481113, 27.32187500034139660, -47.42413220539094709 ) ) ;
#283 = EDGE_CURVE ( 'NONE', #13340, #691, #14944, .T. ) ;
#284 =( BOUNDED_CURVE ( )  B_SPLINE_CURVE ( 2, ( #4150, #13941, #12709, #1308, #6399, #11460, #5161, #10217, #15270, #3902, #8972, #5486, #15612 ),
 .UNSPECIFIED., .F., .T. ) 
 B_SPLINE_CURVE_WITH_KNOTS ( ( 3, 2, 2, 2, 2, 2, 3 ),
 ( 0.1166666666666666685, 0.1199999999999999956, 0.1266666666666666774, 0.1333333333333333315, 0.1400000000000000133, 0.1466666666666666674, 0.1499999999999999944 ),
 .UNSPECIFIED. ) 
 CURVE ( )  GEOMETRIC_REPRESENTATION_ITEM ( )  RATIONAL_B_SPLINE_CURVE ( ( 0.9755282581475768211, 0.9755282581475768211, 1.000000000000000000, 0.9510565162951535312, 1.000000000000000000, 0.9510565162951535312, 1.000000000000000000, 0.9510565162951535312, 1.000000000000000000, 0.9510565162951535312, 1.000000000000000000, 0.9755282581475768211, 0.9755282581475768211 ) ) 
 REPRESENTATION_ITEM ( '' )  );
#285 = CARTESIAN_POINT ( 'NONE',  ( -30.90169943749474513, 27.70000000000000284, -42.53254041760200721 ) ) ;
#286 = VERTEX_POINT ( 'NONE', #8651 ) ;
#287 = CARTESIAN_POINT ( 'NONE',  ( 30.90169943749475578, 34.48125000068279888, 42.53254041760200010 ) ) ;
#288 = ORIENTED_EDGE ( 'NONE', *, *, #496, .T. ) ;
#289 = FACE_OUTER_BOUND ( 'NONE', #4833, .T. ) ;
#290 = LINE ( 'NONE', #6642, #14465 ) ;
#291 = DIRECTION ( 'NONE',  ( 0.000000000000000000, 0.000000000000000000, 1.000000000000000000 ) ) ;
#292 = CARTESIAN_POINT ( 'NONE',  ( 49.86468353125000164, 48.92187500034139447, -6.106662507704105588E-15 ) ) ;
#293 = CARTESIAN_POINT ( 'NONE',  ( -40.34137639590981195, 28.05937500034139731, 29.30972558990012189 ) ) ;
#294 = EDGE_CURVE ( 'NONE', #4877, #10001, #5939, .T. ) ;
#295 = PRODUCT_DEFINITION ( 'UNKNOWN', '', #14486, #8928 ) ;
#296 = DIRECTION ( 'NONE',  ( 0.000000000000000000, -0.7071067811865487940, -0.7071067811865463515 ) ) ;
#297 = CARTESIAN_POINT ( 'NONE',  ( 15.40903463028482356, 40.52187500034139589, 47.42413220539093999 ) ) ;
#298 = DIRECTION ( 'NONE',  ( 1.000000000000000000, 0.000000000000000000, 0.000000000000000000 ) ) ;
#299 = CARTESIAN_POINT ( 'NONE',  ( 40.45084971874737079, 34.98125000068279888, -29.38926261462366440 ) ) ;
#300 = CARTESIAN_POINT ( 'NONE',  ( 49.86468353125001585, 48.82187500034139305, 16.20201782572375038 ) ) ;
#301 = DIRECTION ( 'NONE',  ( 0.9945218953682730678, 0.1045284632676572456, 0.000000000000000000 ) ) ;
#302 = ORIENTED_EDGE ( 'NONE', *, *, #6524, .T. ) ;
#303 = CARTESIAN_POINT ( 'NONE',  ( 9.631387414534489405E-15, 48.42187500034140157, 52.43083105670540789 ) ) ;
#304 = ORIENTED_EDGE ( 'NONE', *, *, #3039, .T. ) ;
#305 = VERTEX_POINT ( 'NONE', #3593 ) ;
#306 = VERTEX_POINT ( 'NONE', #6172 ) ;
#307 = EDGE_CURVE ( 'NONE', #2544, #15408, #9753, .T. ) ;
#308 = CARTESIAN_POINT ( 'NONE',  ( -40.45084971874737789, 43.58125000068280031, -29.38926261462365730 ) ) ;
#309 = FACE_OUTER_BOUND ( 'NONE', #6282, .T. ) ;
#310 = CARTESIAN_POINT ( 'NONE',  ( 0.000000000000000000, 22.50000000000000000, 102.0000000000000142 ) ) ;
#311 = CARTESIAN_POINT ( 'NONE',  ( 50.00000000000000711, 24.90000000000000213, 16.24598481164530739 ) ) ;
#312 = CARTESIAN_POINT ( 'NONE',  ( 49.86468353125000164, 42.85937500034140157, -6.106662507704105588E-15 ) ) ;
#313 = DIRECTION ( 'NONE',  ( 0.000000000000000000, 0.000000000000000000, 1.000000000000000000 ) ) ;
#314 = DIRECTION ( 'NONE',  ( 0.000000000000000000, -1.000000000000000000, 0.000000000000000000 ) ) ;
#315 = CARTESIAN_POINT ( 'NONE',  ( 49.86468353125000164, 20.92187500034139802, -6.106662507704105588E-15 ) ) ;
#316 = SURFACE_SIDE_STYLE ('',( #6586 ) ) ;
#317 = DIRECTION ( 'NONE',  ( 0.000000000000000000, 0.000000000000000000, 1.000000000000000000 ) ) ;
#318 = CARTESIAN_POINT ( 'NONE',  ( -15.45084971874736368, 42.18125000068279462, 47.55282581475768211 ) ) ;
#319 = CARTESIAN_POINT ( 'NONE',  ( 1.293669679204937499E-13, 37.28125000068280315, -50.00000000000000000 ) ) ;
#320 = EDGE_CURVE ( 'NONE', #5080, #1275, #14407, .T. ) ;
#321 = CARTESIAN_POINT ( 'NONE',  ( -0.1743114854953159432, 100.0076106038165165, -5.000000000000000000 ) ) ;
#322 = CARTESIAN_POINT ( 'NONE',  ( -6.522576737113937817, 38.37924387995715847, 101.3333374614808662 ) ) ;
#323 = ORIENTED_EDGE ( 'NONE', *, *, #16173, .F. ) ;
#324 = CARTESIAN_POINT ( 'NONE',  ( -49.86468353125000164, 39.85937500034139447, 0.000000000000000000 ) ) ;
#325 = ORIENTED_EDGE ( 'NONE', *, *, #9057, .T. ) ;
#326 = VERTEX_POINT ( 'NONE', #10076 ) ;
#327 = CARTESIAN_POINT ( 'NONE',  ( -50.00000000000000000, 47.78125000068279604, 0.000000000000000000 ) ) ;
#328 = CARTESIAN_POINT ( 'NONE',  ( 4.127528389677815213, 5.486372832567310454, 102.0000000000000142 ) ) ;
#330 = CARTESIAN_POINT ( 'NONE',  ( -15.40903463028480580, 20.25937500034139660, 47.42413220539094709 ) ) ;
#329 = SHAPE_REPRESENTATION ( 'lid', ( #15812 ), #9193 ) ;
#332 = VERTEX_POINT ( 'NONE', #9993 ) ;
#331 = VECTOR ( 'NONE', #11777, 1000.000000000000000 ) ;
#333 = DIRECTION ( 'NONE',  ( 0.000000000000000000, 1.000000000000000000, 0.000000000000000000 ) ) ;
#334 = CARTESIAN_POINT ( 'NONE',  ( 50.00000000000000711, 22.89999999999999858, 16.24598481164530739 ) ) ;
#335 = DIRECTION ( 'NONE',  ( -5.069245582283711292E-17, -1.000000000000000000, 8.780190904559502465E-17 ) ) ;
#336 = CARTESIAN_POINT ( 'NONE',  ( 40.34137639590981195, 27.12187500034139731, -29.30972558990011834 ) ) ;
#337 = DIRECTION ( 'NONE',  ( 1.000000000000000000, 0.000000000000000000, 0.000000000000000000 ) ) ;
#338 = DIRECTION ( 'NONE',  ( 1.000000000000000000, 3.291018251567428497E-14, 0.000000000000000000 ) ) ;
#339 = CARTESIAN_POINT ( 'NONE',  ( -48.15826639445383961, 20.00000000000001066, 12.93428853971354009 ) ) ;
#340 = ADVANCED_FACE ( 'NONE', ( #12408 ), #9995, .T. ) ;
#341 = CARTESIAN_POINT ( 'NONE',  ( -30.81806926056962226, 26.22187500034139518, 42.41743335407647209 ) ) ;
#342 = DIRECTION ( 'NONE',  ( 0.000000000000000000, -0.000000000000000000, 1.000000000000000000 ) ) ;
#343 = CARTESIAN_POINT ( 'NONE',  ( 15.45084971874736723, 35.39999999999999858, -47.55282581475768211 ) ) ;
#344 = CARTESIAN_POINT ( 'NONE',  ( 30.81806926056962936, 35.15937500034139873, -42.41743335407647209 ) ) ;
#345 = AXIS2_PLACEMENT_3D ( 'NONE', #4776, #4685, #917 ) ;
#346 = CARTESIAN_POINT ( 'NONE',  ( 40.45084971874737789, 38.80000000000000426, 29.38926261462365375 ) ) ;
#347 = EDGE_LOOP ( 'NONE', ( #13905, #11587, #8273, #12260 ) ) ;
#348 = CARTESIAN_POINT ( 'NONE',  ( 49.86468353124999453, 26.95937500034139944, -16.20201782572376104 ) ) ;
#349 = ORIENTED_EDGE ( 'NONE', *, *, #7162, .F. ) ;
#350 = DIRECTION ( 'NONE',  ( -0.000000000000000000, -1.000000000000000000, -0.000000000000000000 ) ) ;
#351 = CARTESIAN_POINT ( 'NONE',  ( -49.86468353124999453, 39.95937500034139589, 16.20201782572377525 ) ) ;
#352 = DIRECTION ( 'NONE',  ( 0.000000000000000000, 1.000000000000000000, 0.000000000000000000 ) ) ;
#353 = CARTESIAN_POINT ( 'NONE',  ( 20.51073895446616291, 285.3889217077638705, 7.755369477227151975 ) ) ;
#354 = CARTESIAN_POINT ( 'NONE',  ( -27.49424662897630256, 282.6608420050619088, 7.488493257954157656 ) ) ;
#355 = CARTESIAN_POINT ( 'NONE',  ( 30.81806926056962936, 33.22187500034139163, -42.41743335407647209 ) ) ;
#356 = CARTESIAN_POINT ( 'NONE',  ( 9.631387414534489405E-15, 36.35937500034140157, 52.43083105670540789 ) ) ;
#357 = CARTESIAN_POINT ( 'NONE',  ( 5.000000000000000000, 102.0000000000000142, -7.580410092414002321 ) ) ;
#358 = CARTESIAN_POINT ( 'NONE',  ( -49.99999999999999289, 44.09999999999999432, 16.24598481164533226 ) ) ;
#359 = CARTESIAN_POINT ( 'NONE',  ( 49.86468353125000164, 48.85937500034139447, -6.106662507704105588E-15 ) ) ;
#360 = CARTESIAN_POINT ( 'NONE',  ( -49.86468353124999453, 43.82187500034140015, -16.20201782572375393 ) ) ;
#361 = CARTESIAN_POINT ( 'NONE',  ( 49.86468353125001585, 30.82187500034139660, 16.20201782572375038 ) ) ;
#362 = AXIS2_PLACEMENT_3D ( 'NONE', #15623, #11718, #317 ) ;
#363 = CARTESIAN_POINT ( 'NONE',  ( -15.40903463028480580, 48.25937500034140015, 47.42413220539094709 ) ) ;
#364 = ORIENTED_EDGE ( 'NONE', *, *, #5866, .F. ) ;
#365 = CARTESIAN_POINT ( 'NONE',  ( 9.657523855033129090E-15, 36.28125000068278894, 52.57311121191334990 ) ) ;
#366 = ORIENTED_EDGE ( 'NONE', *, *, #16114, .F. ) ;
#367 = PLANE ( 'NONE',  #5230 ) ;
#368 = CARTESIAN_POINT ( 'NONE',  ( 1.100495818310455813E-14, 282.0000000000000000, -88.87749532708107836 ) ) ;
#369 = CARTESIAN_POINT ( 'NONE',  ( -2.547328955960238000E-13, 30.28125000068279604, 49.99999999999999289 ) ) ;
#370 = CARTESIAN_POINT ( 'NONE',  ( 9.631387414534489405E-15, 44.42187500034140157, 52.43083105670540789 ) ) ;
#371 = CARTESIAN_POINT ( 'NONE',  ( -40.34137639590981905, 27.65937500034139873, -29.30972558990011478 ) ) ;
#372 = CARTESIAN_POINT ( 'NONE',  ( -37.77664397204053159, 25.00000000000000355, -13.15010152849376190 ) ) ;
#373 = VECTOR ( 'NONE', #8711, 1000.000000000000000 ) ;
#374 = CARTESIAN_POINT ( 'NONE',  ( 9.631387414534489405E-15, 40.42187500034138736, 52.43083105670540789 ) ) ;
#375 = DIRECTION ( 'NONE',  ( 0.000000000000000000, 0.000000000000000000, 1.000000000000000000 ) ) ;
#376 = CARTESIAN_POINT ( 'NONE',  ( 0.000000000000000000, 54.99999999999999289, 0.000000000000000000 ) ) ;
#377 = CARTESIAN_POINT ( 'NONE',  ( 15.40903463028481113, 47.32187500034140015, -47.42413220539094709 ) ) ;
#378 = FACE_OUTER_BOUND ( 'NONE', #6121, .T. ) ;
#379 = ORIENTED_EDGE ( 'NONE', *, *, #147, .T. ) ;
#380 = CARTESIAN_POINT ( 'NONE',  ( -49.86468353124999453, 49.82187500034140015, -16.20201782572375393 ) ) ;
#381 = EDGE_LOOP ( 'NONE', ( #515, #9607 ) ) ;
#382 = CARTESIAN_POINT ( 'NONE',  ( 0.000000000000000000, 52.00000000000000711, 0.000000000000000000 ) ) ;
#383 = VERTEX_POINT ( 'NONE', #15129 ) ;
#384 = VERTEX_POINT ( 'NONE', #2495 ) ;
#385 = AXIS2_PLACEMENT_3D ( 'NONE', #4470, #15603, #705 ) ;
#386 = VECTOR ( 'NONE', #2589, 1000.000000000000000 ) ;
#387 = LINE ( 'NONE', #5491, #7888 ) ;
#388 = CARTESIAN_POINT ( 'NONE',  ( -8.660254037844387298, 28.00000000000000355, 5.000000000000000000 ) ) ;
#389 = DIRECTION ( 'NONE',  ( 0.000000000000000000, 0.000000000000000000, 1.000000000000000000 ) ) ;
#390 = CARTESIAN_POINT ( 'NONE',  ( -49.99999999999999289, 26.10000000000000142, 16.24598481164533226 ) ) ;
#391 = CARTESIAN_POINT ( 'NONE',  ( 49.86468353125001585, 42.75937500034138594, 16.20201782572375038 ) ) ;
#392 = CARTESIAN_POINT ( 'NONE',  ( -37.77664397204053159, 40.00000000000000711, -13.15010152849376190 ) ) ;
#393 = CARTESIAN_POINT ( 'NONE',  ( 0.000000000000000000, 193.4213562373095385, -50.00000000000000000 ) ) ;
#394 = CARTESIAN_POINT ( 'NONE',  ( -50.00000000000000000, 33.78125000068280315, 0.000000000000000000 ) ) ;
#395 = LINE ( 'NONE', #4248, #7805 ) ;
#396 = CARTESIAN_POINT ( 'NONE',  ( -40.45084971874737079, 39.98125000068279888, 29.38926261462367151 ) ) ;
#397 = CARTESIAN_POINT ( 'NONE',  ( -1.240322475938754499E-13, 38.28125000068280315, 50.00000000000000000 ) ) ;
#398 = AXIS2_PLACEMENT_3D ( 'NONE', #3986, #3822, #7478 ) ;
#399 = EDGE_CURVE ( 'NONE', #4332, #7924, #11576, .T. ) ;
#400 = CARTESIAN_POINT ( 'NONE',  ( 7.919222016226807881, 46.33250428222964246, 50.00000000000000000 ) ) ;
#401 = COLOUR_RGB ( '', 0.72549020, 0.75294118, 0.79215686) ;
#402 = EDGE_LOOP ( 'NONE', ( #5956, #13937, #15950, #9796 ) ) ;
#403 = CARTESIAN_POINT ( 'NONE',  ( -49.86468353124999453, 39.95937500034139589, 16.20201782572377525 ) ) ;
#404 = VERTEX_POINT ( 'NONE', #14726 ) ;
#405 = ORIENTED_EDGE ( 'NONE', *, *, #8129, .F. ) ;
#406 = ADVANCED_FACE ( 'NONE', ( #16070 ), #6031, .F. ) ;
#407 = EDGE_CURVE ( 'NONE', #5908, #14317, #4415, .T. ) ;
#408 = CARTESIAN_POINT ( 'NONE',  ( 40.45084971874737079, 43.20000000000000284, -29.38926261462366440 ) ) ;
#409 = CIRCLE ( 'NONE', #13951, 40.00000000000000000 ) ;
#410 = VECTOR ( 'NONE', #1881, 1000.000000000000000 ) ;
#411 = DIRECTION ( 'NONE',  ( -1.000000000000000000, 0.000000000000000000, 2.312964634635742464E-16 ) ) ;
#412 = CARTESIAN_POINT ( 'NONE',  ( -15.40903463028480580, 22.25937500034139660, 47.42413220539094709 ) ) ;
#413 = AXIS2_PLACEMENT_3D ( 'NONE', #15842, #2171, #16155 ) ;
#414 = ORIENTED_EDGE ( 'NONE', *, *, #3877, .F. ) ;
#415 = ADVANCED_FACE ( 'NONE', ( #16162 ), #4535, .F. ) ;
#416 = DIRECTION ( 'NONE',  ( -0.3420201433256697121, -0.6644630243886754384, 0.6644630243886734400 ) ) ;
#417 = CARTESIAN_POINT ( 'NONE',  ( 30.90169943749473802, 35.29999999999999716, -42.53254041760200721 ) ) ;
#418 = CARTESIAN_POINT ( 'NONE',  ( -40.34137639590981195, 42.05937500034139731, 29.30972558990012189 ) ) ;
#419 = DIRECTION ( 'NONE',  ( 1.224646799147349509E-16, 0.000000000000000000, -1.000000000000000000 ) ) ;
#420 = CARTESIAN_POINT ( 'NONE',  ( -3.210462471511496205E-15, 27.42187500034139092, -52.43083105670540789 ) ) ;
#421 = CARTESIAN_POINT ( 'NONE',  ( -5.823736356558309156E-14, 44.50000000000000000, 50.00000000000000000 ) ) ;
#422 = CARTESIAN_POINT ( 'NONE',  ( 1.235979693235591175E-19, 4.999999999999997335, 99.11836509645767990 ) ) ;
#423 = CARTESIAN_POINT ( 'NONE',  ( -48.02615145421049903, 20.00000000000000355, 13.41652781627881375 ) ) ;
#424 = CARTESIAN_POINT ( 'NONE',  ( -30.81806926056962226, 32.22187500034139163, 42.41743335407647209 ) ) ;
#425 = CARTESIAN_POINT ( 'NONE',  ( -2.547328955960238000E-13, 22.49999999999999645, 49.99999999999999289 ) ) ;
#426 = CIRCLE ( 'NONE', #15019, 62.25100647794772613 ) ;
#427 = CARTESIAN_POINT ( 'NONE',  ( 40.45084971874737789, 34.80000000000000426, 29.38926261462365375 ) ) ;
#428 = CARTESIAN_POINT ( 'NONE',  ( 9.631387414534489405E-15, 32.35937500034139447, 52.43083105670540789 ) ) ;
#429 = CIRCLE ( 'NONE', #8137, 79.49773270518484480 ) ;
#430 = VECTOR ( 'NONE', #7991, 1000.000000000000000 ) ;
#431 = VECTOR ( 'NONE', #921, 1000.000000000000114 ) ;
#432 = CARTESIAN_POINT ( 'NONE',  ( 49.99999999999999289, 39.10000000000000142, -16.24598481164532160 ) ) ;
#433 = ORIENTED_EDGE ( 'NONE', *, *, #9568, .T. ) ;
#434 =( BOUNDED_CURVE ( )  B_SPLINE_CURVE ( 2, ( #3419, #3668, #8482, #2153, #8725, #747, #10898 ),
 .UNSPECIFIED., .F., .F. ) 
 B_SPLINE_CURVE_WITH_KNOTS ( ( 3, 2, 2, 3 ),
 ( 0.9833333333333333925, 0.9866666666666666918, 0.9933333333333332904, 1.000000000000000000 ),
 .UNSPECIFIED. ) 
 CURVE ( )  GEOMETRIC_REPRESENTATION_ITEM ( )  RATIONAL_B_SPLINE_CURVE ( ( 0.9755282581475768211, 0.9755282581475771542, 1.000000000000000000, 0.9510565162951535312, 1.000000000000000000, 0.9510565162951535312, 1.000000000000000000 ) ) 
 REPRESENTATION_ITEM ( '' )  );
#435 = CARTESIAN_POINT ( 'NONE',  ( -15.40903463028481646, 29.45937500034139589, -47.42413220539093999 ) ) ;
#436 = VERTEX_POINT ( 'NONE', #8430 ) ;
#437 = CARTESIAN_POINT ( 'NONE',  ( 9.234334497652928468E-15, 101.0808929720139702, -9.080892972013931086 ) ) ;
#438 = CARTESIAN_POINT ( 'NONE',  ( 15.40903463028482356, 42.45937500034140299, 47.42413220539093999 ) ) ;
#439 = CARTESIAN_POINT ( 'NONE',  ( -3.111920190527341144E-15, 27.50000000000000000, -50.00000000000000000 ) ) ;
#440 = CARTESIAN_POINT ( 'NONE',  ( 9.631387414534489405E-15, 20.42187500034139802, 52.43083105670540789 ) ) ;
#441 = EDGE_CURVE ( 'NONE', #7797, #13296, #9208, .T. ) ;
#442 = AXIS2_PLACEMENT_3D ( 'NONE', #8820, #13970, #6598 ) ;
#443 = CARTESIAN_POINT ( 'NONE',  ( -30.00000000000000711, 282.0000000000000000, 12.50000000000000000 ) ) ;
#444 = CARTESIAN_POINT ( 'NONE',  ( -40.34137639590981905, 37.72187500034139873, -29.30972558990011478 ) ) ;
#445 = CARTESIAN_POINT ( 'NONE',  ( -15.40903463028481646, 35.45937500034139589, -47.42413220539093999 ) ) ;
#446 = DIRECTION ( 'NONE',  ( 0.1045284632676572456, -0.9945218953682730678, -0.000000000000000000 ) ) ;
#447 = CARTESIAN_POINT ( 'NONE',  ( -30.90169943749473802, 44.30000000000001137, 42.53254041760200721 ) ) ;
#448 = CARTESIAN_POINT ( 'NONE',  ( -15.40903463028481646, 49.45937500034140299, -47.42413220539093999 ) ) ;
#449 = CARTESIAN_POINT ( 'NONE',  ( 15.40903463028482356, 42.52187500034139589, 47.42413220539093999 ) ) ;
#450 = CARTESIAN_POINT ( 'NONE',  ( -3.210462471511496205E-15, 25.42187500034139092, -52.43083105670540789 ) ) ;
#451 = AXIS2_PLACEMENT_3D ( 'NONE', #16347, #7624, #4984 ) ;
#452 = CARTESIAN_POINT ( 'NONE',  ( -40.45084971874737789, 27.58125000068280031, -29.38926261462365730 ) ) ;
#453 = ORIENTED_EDGE ( 'NONE', *, *, #626, .F. ) ;
#454 = CARTESIAN_POINT ( 'NONE',  ( 50.00000000000000000, 30.78125000068279959, -6.123233995736766085E-15 ) ) ;
#455 = EDGE_LOOP ( 'NONE', ( #15919, #7029, #1227 ) ) ;
#456 = CARTESIAN_POINT ( 'NONE',  ( -7.580410092413954359, 101.3368000520362813, 5.000000000000000000 ) ) ;
#457 = CARTESIAN_POINT ( 'NONE',  ( 9.574901606694759531E-15, 52.00000000000001421, -2.191293403013901479E-14 ) ) ;
#458 = CARTESIAN_POINT ( 'NONE',  ( -40.45084971874737079, 33.98125000068279888, 29.38926261462367151 ) ) ;
#459 = CARTESIAN_POINT ( 'NONE',  ( 30.81806926056964002, 46.62187500034139731, 42.41743335407646498 ) ) ;
#460 = ADVANCED_FACE ( 'NONE', ( #10847 ), #14901, .F. ) ;
#461 = CARTESIAN_POINT ( 'NONE',  ( -49.86468353124999453, 27.95937500034139944, 16.20201782572377525 ) ) ;
#462 = DIRECTION ( 'NONE',  ( 1.000000000000000000, 0.000000000000000000, 0.000000000000000000 ) ) ;
#463 = CARTESIAN_POINT ( 'NONE',  ( -49.86468353124999453, 41.82187500034140015, -16.20201782572375393 ) ) ;
#464 = PRODUCT_CONTEXT ( 'NONE', #15229, 'mechanical' ) ;
#465 = CARTESIAN_POINT ( 'NONE',  ( 30.81806926056964002, 46.62187500034140442, 42.41743335407647209 ) ) ;
#466 = DIRECTION ( 'NONE',  ( 0.000000000000000000, 0.000000000000000000, -1.000000000000000000 ) ) ;
#467 = ORIENTED_EDGE ( 'NONE', *, *, #5813, .T. ) ;
#468 = CARTESIAN_POINT ( 'NONE',  ( -40.34137639590981905, 49.72187500034139873, -29.30972558990011478 ) ) ;
#469 = ORIENTED_EDGE ( 'NONE', *, *, #407, .T. ) ;
#470 = ORIENTED_EDGE ( 'NONE', *, *, #10226, .T. ) ;
#471 =( REPRESENTATION_RELATIONSHIP ('NONE','NONE', #6178, #13496 ) REPRESENTATION_RELATIONSHIP_WITH_TRANSFORMATION ( #9695 )SHAPE_REPRESENTATION_RELATIONSHIP( ) );
#472 = CARTESIAN_POINT ( 'NONE',  ( 0.000000000000000000, 22.50000000000000000, 80.00000000000000000 ) ) ;
#473 = CARTESIAN_POINT ( 'NONE',  ( 5.000000000000000000, 92.00000000000001421, 0.000000000000000000 ) ) ;
#474 = DIRECTION ( 'NONE',  ( -0.000000000000000000, -0.000000000000000000, 1.000000000000000000 ) ) ;
#475 = CARTESIAN_POINT ( 'NONE',  ( 9.657523855033129090E-15, 24.50000000000000355, 52.57311121191334990 ) ) ;
#476 = CARTESIAN_POINT ( 'NONE',  ( -3.210462471511496205E-15, 47.35937500034138736, -52.43083105670540789 ) ) ;
#477 = DIRECTION ( 'NONE',  ( 0.9361168066628590134, -0.08189960831908912886, 0.3420201433256691570 ) ) ;
#478 = CARTESIAN_POINT ( 'NONE',  ( 0.5000000000000000000, 242.0000000000000284, -49.99999999999999289 ) ) ;
#479 = VECTOR ( 'NONE', #830, 1000.000000000000000 ) ;
#480 = AXIS2_PLACEMENT_3D ( 'NONE', #4431, #4348, #13149 ) ;
#481 = FILL_AREA_STYLE_COLOUR ( '', #401 ) ;
#482 = LINE ( 'NONE', #8144, #13108 ) ;
#483 = CARTESIAN_POINT ( 'NONE',  ( -15.45084971874736368, 32.18125000068279462, 47.55282581475768211 ) ) ;
#484 = CARTESIAN_POINT ( 'NONE',  ( 24.78626291527386272, 25.00000000000000355, -5.650101528494135827 ) ) ;
#485 = PLANE ( 'NONE',  #8421 ) ;
#486 = CARTESIAN_POINT ( 'NONE',  ( 8.446640517145639571E-15, 26.28125000068279959, 50.00000000000000000 ) ) ;
#487 = ORIENTED_EDGE ( 'NONE', *, *, #6442, .T. ) ;
#488 = CARTESIAN_POINT ( 'NONE',  ( 15.40903463028481113, 37.25937500034140015, -47.42413220539094709 ) ) ;
#489 = ORIENTED_EDGE ( 'NONE', *, *, #10675, .F. ) ;
#490 = ORIENTED_EDGE ( 'NONE', *, *, #10727, .F. ) ;
#491 = CARTESIAN_POINT ( 'NONE',  ( -15.45084971874736368, 48.18125000068280173, 47.55282581475768211 ) ) ;
#492 = AXIS2_PLACEMENT_3D ( 'NONE', #10068, #2407, #11397 ) ;
#493 = DIRECTION ( 'NONE',  ( -0.3535533905932818355, -0.7071067811865463515, -0.6123724356957914727 ) ) ;
#494 = CARTESIAN_POINT ( 'NONE',  ( -49.86468353124999453, 23.75937500034140015, -16.20201782572375393 ) ) ;
#495 = VERTEX_POINT ( 'NONE', #2020 ) ;
#496 = EDGE_CURVE ( 'NONE', #9157, #8721, #11184, .T. ) ;
#497 = CARTESIAN_POINT ( 'NONE',  ( -30.90169943749474513, 47.70000000000000284, -42.53254041760200721 ) ) ;
#498 = CARTESIAN_POINT ( 'NONE',  ( 40.45084971874737079, 23.20000000000000284, -29.38926261462366440 ) ) ;
#499 = FACE_OUTER_BOUND ( 'NONE', #6302, .T. ) ;
#500 = CARTESIAN_POINT ( 'NONE',  ( -3.210462471511496205E-15, 25.42187500034139447, -52.43083105670540789 ) ) ;
#501 = CARTESIAN_POINT ( 'NONE',  ( -30.90169943749473447, 30.08125000068279675, 42.53254041760200721 ) ) ;
#502 = DIRECTION ( 'NONE',  ( -0.8660254037844433705, 0.4999999999999918399, 0.000000000000000000 ) ) ;
#503 = ADVANCED_FACE ( 'NONE', ( #9598 ), #12925, .T. ) ;
#504 = CARTESIAN_POINT ( 'NONE',  ( -47.65000835890729292, 20.00000000000000355, 14.69569212619059684 ) ) ;
#505 = CARTESIAN_POINT ( 'NONE',  ( 30.81806926056962936, 23.22187500034139163, -42.41743335407646498 ) ) ;
#506 = ADVANCED_FACE ( 'NONE', ( #2101 ), #15988, .T. ) ;
#507 = FACE_OUTER_BOUND ( 'NONE', #6954, .T. ) ;
#508 = CIRCLE ( 'NONE', #13785, 50.00000000000000000 ) ;
#509 = CARTESIAN_POINT ( 'NONE',  ( 15.45084971874737789, 32.60000000000000142, 47.55282581475767500 ) ) ;
#510 = CARTESIAN_POINT ( 'NONE',  ( 40.34137639590981905, 34.65937500034139873, 29.30972558990010768 ) ) ;
#511 = CARTESIAN_POINT ( 'NONE',  ( 1.293669679204937499E-13, 41.28125000068279604, -50.00000000000000000 ) ) ;
#512 = EDGE_CURVE ( 'NONE', #3799, #13515, #6038, .T. ) ;
#513 = ORIENTED_EDGE ( 'NONE', *, *, #11703, .T. ) ;
#514 = CARTESIAN_POINT ( 'NONE',  ( 40.34137639590981195, 27.05937500034139731, -29.30972558990011834 ) ) ;
#515 = ORIENTED_EDGE ( 'NONE', *, *, #6228, .F. ) ;
#516 = CARTESIAN_POINT ( 'NONE',  ( 43.87482193696061472, 262.0000000000000000, -10.00000000000000000 ) ) ;
#517 = CARTESIAN_POINT ( 'NONE',  ( 49.86468353125000164, 40.85937500034139447, -6.106662507704105588E-15 ) ) ;
#518 = ADVANCED_FACE ( 'NONE', ( #4613 ), #3612, .F. ) ;
#519 = VECTOR ( 'NONE', #4561, 1000.000000000000000 ) ;
#520 = CARTESIAN_POINT ( 'NONE',  ( 22.04892374372132835, 283.9500510409123422, 8.524461871856116701 ) ) ;
#521 = CARTESIAN_POINT ( 'NONE',  ( -29.34550962211183744, 282.0322304394514390, 11.19101924422352212 ) ) ;
#522 = CARTESIAN_POINT ( 'NONE',  ( -49.86468353125000164, 37.92187500034140157, 0.000000000000000000 ) ) ;
#523 = CARTESIAN_POINT ( 'NONE',  ( -30.81806926056963292, 37.55937500034139020, -42.41743335407646498 ) ) ;
#524 = DIRECTION ( 'NONE',  ( -0.8660254037844399289, 0.000000000000000000, -0.4999999999999976685 ) ) ;
#525 = CARTESIAN_POINT ( 'NONE',  ( -40.45084971874737079, 40.20000000000000284, 29.38926261462367151 ) ) ;
#526 = CARTESIAN_POINT ( 'NONE',  ( 15.45084971874736723, 23.18125000068279817, -47.55282581475768211 ) ) ;
#527 = CARTESIAN_POINT ( 'NONE',  ( 15.40903463028481113, 47.32187500034140015, -47.42413220539094709 ) ) ;
#528 =( BOUNDED_CURVE ( )  B_SPLINE_CURVE ( 2, ( #2578, #6411, #11472, #156, #11398, #69, #5174 ),
 .UNSPECIFIED., .F., .F. ) 
 B_SPLINE_CURVE_WITH_KNOTS ( ( 3, 2, 2, 3 ),
 ( 0.000000000000000000, 0.006666666666666667095, 0.01333333333333333419, 0.01666666666666666990 ),
 .UNSPECIFIED. ) 
 CURVE ( )  GEOMETRIC_REPRESENTATION_ITEM ( )  RATIONAL_B_SPLINE_CURVE ( ( 1.000000000000000000, 0.9510565162951535312, 1.000000000000000000, 0.9510565162951535312, 1.000000000000000000, 0.9755282581475768211, 0.9755282581475768211 ) ) 
 REPRESENTATION_ITEM ( '' )  );
#529 = ADVANCED_FACE ( 'NONE', ( #2178 ), #12250, .T. ) ;
#530 = CARTESIAN_POINT ( 'NONE',  ( 49.86468353125000164, 26.92187500034139802, -6.106662507704105588E-15 ) ) ;
#531 = CARTESIAN_POINT ( 'NONE',  ( 15.40903463028481113, 47.25937500034140015, -47.42413220539094709 ) ) ;
#532 = VERTEX_POINT ( 'NONE', #12078 ) ;
#534 = EDGE_CURVE ( 'NONE', #9508, #1121, #9961, .T. ) ;
#533 = CARTESIAN_POINT ( 'NONE',  ( 50.00000000000000000, 32.78125000068279604, -6.123233995736766085E-15 ) ) ;
#535 = ORIENTED_EDGE ( 'NONE', *, *, #3544, .T. ) ;
#536 = DIRECTION ( 'NONE',  ( 0.000000000000000000, -1.541976423090494894E-16, -1.000000000000000000 ) ) ;
#537 = DIRECTION ( 'NONE',  ( -0.000000000000000000, -0.6143407043256620126, -0.7890408728378077718 ) ) ;
#538 = CARTESIAN_POINT ( 'NONE',  ( 40.34137639590981195, 43.12187500034139731, -29.30972558990011834 ) ) ;
#539 = CARTESIAN_POINT ( 'NONE',  ( -40.34137639590981195, 26.05937500034139731, 29.30972558990012189 ) ) ;
#540 = FACE_OUTER_BOUND ( 'NONE', #4983, .T. ) ;
#541 = CARTESIAN_POINT ( 'NONE',  ( -30.81806926056963292, 39.62187500034139020, -42.41743335407646498 ) ) ;
#542 = APPLICATION_PROTOCOL_DEFINITION ( 'draft international standard', 'automotive_design', 1998, #13231 ) ;
#543 = CARTESIAN_POINT ( 'NONE',  ( -3.210462471511496205E-15, 49.42187500034138736, -52.43083105670540789 ) ) ;
#544 = DIRECTION ( 'NONE',  ( 1.000000000000000000, 0.000000000000000000, 0.000000000000000000 ) ) ;
#545 = ORIENTED_EDGE ( 'NONE', *, *, #14628, .F. ) ;
#546 = CARTESIAN_POINT ( 'NONE',  ( -30.81806926056963292, 41.62187500034139020, -42.41743335407647209 ) ) ;
#547 = PRODUCT_DEFINITION_SHAPE ( 'NONE', 'NONE',  #11888 ) ;
#548 = ORIENTED_EDGE ( 'NONE', *, *, #4265, .T. ) ;
#549 = ORIENTED_EDGE ( 'NONE', *, *, #13824, .F. ) ;
#550 = DIRECTION ( 'NONE',  ( 0.000000000000000000, 1.000000000000000000, 0.000000000000000000 ) ) ;
#551 = LINE ( 'NONE', #10709, #923 ) ;
#552 = DIRECTION ( 'NONE',  ( 0.000000000000000000, -1.000000000000000000, 0.000000000000000000 ) ) ;
#553 = CARTESIAN_POINT ( 'NONE',  ( -40.45084971874737789, 25.80000000000000071, -29.38926261462365730 ) ) ;
#554 = CARTESIAN_POINT ( 'NONE',  ( -40.34137639590981905, 45.65937500034139873, -29.30972558990011478 ) ) ;
#555 = CARTESIAN_POINT ( 'NONE',  ( -30.81806926056963292, 47.55937500034139731, -42.41743335407646498 ) ) ;
#556 = CARTESIAN_POINT ( 'NONE',  ( -2.547328955960238000E-13, 32.28125000068278894, 49.99999999999999289 ) ) ;
#557 = LINE ( 'NONE', #12035, #8938 ) ;
#558 = CARTESIAN_POINT ( 'NONE',  ( 1.875620865444973696E-15, 37.00000000000001421, -3.248670634687016947E-15 ) ) ;
#559 = LINE ( 'NONE', #811, #4989 ) ;
#560 = CARTESIAN_POINT ( 'NONE',  ( 40.45084971874737789, 22.58125000068279675, 29.38926261462365375 ) ) ;
#561 = CARTESIAN_POINT ( 'NONE',  ( 40.45084971874737789, 36.79999999999999716, 29.38926261462365375 ) ) ;
#562 = VERTEX_POINT ( 'NONE', #6435 ) ;
#563 = CARTESIAN_POINT ( 'NONE',  ( -49.86468353124999453, 31.75937500034140015, -16.20201782572375393 ) ) ;
#564 = EDGE_CURVE ( 'NONE', #10216, #11191, #8756, .T. ) ;
#565 = ORIENTED_EDGE ( 'NONE', *, *, #14515, .F. ) ;
#566 = VERTEX_POINT ( 'NONE', #11495 ) ;
#567 = EDGE_LOOP ( 'NONE', ( #8568, #5125, #571, #2717, #7157 ) ) ;
#568 = CARTESIAN_POINT ( 'NONE',  ( 0.000000000000000000, 20.00000000000000355, 0.000000000000000000 ) ) ;
#569 = CARTESIAN_POINT ( 'NONE',  ( 4.000000000000001776, 22.50000000000000000, 101.0000000000000000 ) ) ;
#570 = CARTESIAN_POINT ( 'NONE',  ( 40.34137639590981905, 22.65937500034139518, 29.30972558990010768 ) ) ;
#571 = ORIENTED_EDGE ( 'NONE', *, *, #12236, .F. ) ;
#572 = LINE ( 'NONE', #1986, #430 ) ;
#573 = CARTESIAN_POINT ( 'NONE',  ( 48.98979485566356118, 261.9999999999999432, -10.00000000000000178 ) ) ;
#574 = DIRECTION ( 'NONE',  ( 0.000000000000000000, 0.000000000000000000, -1.000000000000000000 ) ) ;
#575 = CARTESIAN_POINT ( 'NONE',  ( 15.40903463028482356, 30.52187500034139589, 47.42413220539093999 ) ) ;
#576 = DIRECTION ( 'NONE',  ( -0.000000000000000000, -1.000000000000000000, -0.000000000000000000 ) ) ;
#577 = EDGE_CURVE ( 'NONE', #11849, #532, #92, .T. ) ;
#578 = CARTESIAN_POINT ( 'NONE',  ( 13.94233552421758837, 11.90832207049870206, 96.90308138387069903 ) ) ;
#579 = LINE ( 'NONE', #1757, #15758 ) ;
#580 = CARTESIAN_POINT ( 'NONE',  ( -40.34137639590981195, 22.12187500034139731, 29.30972558990012189 ) ) ;
#581 = FACE_BOUND ( 'NONE', #14554, .T. ) ;
#582 = CARTESIAN_POINT ( 'NONE',  ( -49.99999999999999289, 35.90000000000000568, -16.24598481164531449 ) ) ;
#583 = CARTESIAN_POINT ( 'NONE',  ( 49.86468353125001585, 28.75937500034139305, 16.20201782572375038 ) ) ;
#584 = CARTESIAN_POINT ( 'NONE',  ( -40.34137639590981905, 47.65937500034139873, -29.30972558990011478 ) ) ;
#585 = ORIENTED_EDGE ( 'NONE', *, *, #16374, .T. ) ;
#586 = AXIS2_PLACEMENT_3D ( 'NONE', #1715, #3134, #466 ) ;
#587 = UNCERTAINTY_MEASURE_WITH_UNIT (LENGTH_MEASURE( 1.000000000000000082E-05 ), #11527, 'distance_accuracy_value', 'NONE');
#588 = CARTESIAN_POINT ( 'NONE',  ( 15.40903463028482356, 28.45937500034139589, 47.42413220539093999 ) ) ;
#589 = VERTEX_POINT ( 'NONE', #13983 ) ;
#590 = EDGE_CURVE ( 'NONE', #9937, #12980, #2354, .T. ) ;
#591 = CARTESIAN_POINT ( 'NONE',  ( 0.000000000000000000, 20.00000000000000355, 0.000000000000000000 ) ) ;
#592 = CARTESIAN_POINT ( 'NONE',  ( 30.81806926056962936, 41.15937500034139873, -42.41743335407647209 ) ) ;
#593 = CARTESIAN_POINT ( 'NONE',  ( 28.07127062163604947, 282.3184422169448453, 10.57127062163685949 ) ) ;
#594 = CARTESIAN_POINT ( 'NONE',  ( -27.61612561546114009, 282.5087415087664908, 10.11612561546189681 ) ) ;
#595 = CARTESIAN_POINT ( 'NONE',  ( -49.86468353125000164, 29.92187500034139802, 0.000000000000000000 ) ) ;
#596 = CARTESIAN_POINT ( 'NONE',  ( -49.86468353125000164, 37.85937500034139447, 0.000000000000000000 ) ) ;
#597 = CARTESIAN_POINT ( 'NONE',  ( -8.477241335952138357, 18.18301270189218855, 101.0000000000000000 ) ) ;
#598 = CARTESIAN_POINT ( 'NONE',  ( 30.81806926056962936, 31.22187500034139873, -42.41743335407647209 ) ) ;
#599 = CARTESIAN_POINT ( 'NONE',  ( 30.90169943749474157, 39.30000000000000426, -42.53254041760200721 ) ) ;
#600 = AXIS2_PLACEMENT_3D ( 'NONE', #14454, #6924, #1670 ) ;
#601 = CARTESIAN_POINT ( 'NONE',  ( -3.210462471511496205E-15, 47.35937500034138736, -52.43083105670540789 ) ) ;
#602 = CARTESIAN_POINT ( 'NONE',  ( -49.86468353124999453, 46.02187500034140299, 16.20201782572377525 ) ) ;
#603 = EDGE_CURVE ( 'NONE', #14587, #8799, #10009, .T. ) ;
#604 = CARTESIAN_POINT ( 'NONE',  ( -15.40903463028481646, 23.52187500034139944, -47.42413220539093999 ) ) ;
#605 = VERTEX_POINT ( 'NONE', #11575 ) ;
#606 = EDGE_CURVE ( 'NONE', #16014, #2610, #15398, .T. ) ;
#607 = CARTESIAN_POINT ( 'NONE',  ( -15.45084971874736368, 28.18125000068279817, 47.55282581475768211 ) ) ;
#608 = ORIENTED_EDGE ( 'NONE', *, *, #2441, .T. ) ;
#609 = CARTESIAN_POINT ( 'NONE',  ( -40.45084971874737079, 29.98125000068279888, 29.38926261462367151 ) ) ;
#610 = CIRCLE ( 'NONE', #11775, 50.00000000000000000 ) ;
#611 = EDGE_LOOP ( 'NONE', ( #10773, #246, #14152, #10214 ) ) ;
#612 = CARTESIAN_POINT ( 'NONE',  ( -5.823736356558309156E-14, 44.28125000068280315, 50.00000000000000000 ) ) ;
#613 = ADVANCED_FACE ( 'NONE', ( #11344 ), #15222, .F. ) ;
#614 = CARTESIAN_POINT ( 'NONE',  ( -30.81806926056963292, 39.62187500034139020, -42.41743335407646498 ) ) ;
#615 = CARTESIAN_POINT ( 'NONE',  ( 49.86468353125000164, 20.85937500034139802, -6.106662507704105588E-15 ) ) ;
#616 = DIRECTION ( 'NONE',  ( 0.8660254037844398178, 0.000000000000000000, 0.4999999999999978351 ) ) ;
#617 =( BOUNDED_CURVE ( )  B_SPLINE_CURVE ( 2, ( #7741, #2667, #10000, #7663, #1411, #169, #5273, #15383, #8818, #9075, #12734, #16306, #7495 ),
 .UNSPECIFIED., .F., .F. ) 
 B_SPLINE_CURVE_WITH_KNOTS ( ( 3, 2, 2, 2, 2, 2, 3 ),
 ( 0.2166666666666666741, 0.2200000000000000011, 0.2266666666666666552, 0.2333333333333333370, 0.2399999999999999911, 0.2466666666666666730, 0.2500000000000000000 ),
 .UNSPECIFIED. ) 
 CURVE ( )  GEOMETRIC_REPRESENTATION_ITEM ( )  RATIONAL_B_SPLINE_CURVE ( ( 0.9755282581475768211, 0.9755282581475768211, 1.000000000000000000, 0.9510565162951535312, 1.000000000000000000, 0.9510565162951535312, 1.000000000000000000, 0.9510565162951535312, 1.000000000000000000, 0.9510565162951535312, 1.000000000000000000, 0.9755282581475768211, 0.9755282581475765991 ) ) 
 REPRESENTATION_ITEM ( '' )  );
#618 = CARTESIAN_POINT ( 'NONE',  ( 50.00000000000000000, 39.00000000000000000, -6.123233995736766085E-15 ) ) ;
#619 = CIRCLE ( 'NONE', #8873, 45.00000000000000000 ) ;
#620 = CARTESIAN_POINT ( 'NONE',  ( 15.40903463028482356, 42.52187500034139589, 47.42413220539093999 ) ) ;
#621 = DIRECTION ( 'NONE',  ( 0.000000000000000000, 0.000000000000000000, 1.000000000000000000 ) ) ;
#622 = EDGE_LOOP ( 'NONE', ( #7600, #10634, #1804, #893 ) ) ;
#623 = CARTESIAN_POINT ( 'NONE',  ( 15.40903463028482356, 40.52187500034139589, 47.42413220539093999 ) ) ;
#624 = ORIENTED_EDGE ( 'NONE', *, *, #14015, .F. ) ;
#625 = ORIENTED_EDGE ( 'NONE', *, *, #15445, .T. ) ;
#626 = EDGE_CURVE ( 'NONE', #4982, #15172, #5286, .T. ) ;
#627 = CARTESIAN_POINT ( 'NONE',  ( -3.111920190527341144E-15, 45.50000000000000000, -50.00000000000000000 ) ) ;
#628 = CARTESIAN_POINT ( 'NONE',  ( -43.87482193696060762, 257.0000000000001137, 10.00000000000000178 ) ) ;
#629 = AXIS2_PLACEMENT_3D ( 'NONE', #8397, #13467, #15658 ) ;
#630 = ADVANCED_FACE ( 'NONE', ( #6188 ), #1425, .F. ) ;
#631 = DIRECTION ( 'NONE',  ( -0.000000000000000000, -1.000000000000000000, -0.000000000000000000 ) ) ;
#632 = CARTESIAN_POINT ( 'NONE',  ( -50.00000000000000000, 20.00000000000000000, 0.000000000000000000 ) ) ;
#633 = CARTESIAN_POINT ( 'NONE',  ( 15.40903463028481113, 43.25937500034139305, -47.42413220539094709 ) ) ;
#634 = CARTESIAN_POINT ( 'NONE',  ( 40.34137639590981195, 47.05937500034140442, -29.30972558990011834 ) ) ;
#635 = CARTESIAN_POINT ( 'NONE',  ( 7.919222016226809657, 25.44874571845315359, -50.00000000000000000 ) ) ;
#636 = CARTESIAN_POINT ( 'NONE',  ( -30.90169943749474513, 45.70000000000000284, -42.53254041760200721 ) ) ;
#637 = CARTESIAN_POINT ( 'NONE',  ( -7.574663982647817484, 38.28367718720760138, 102.0000000000000142 ) ) ;
#638 = CARTESIAN_POINT ( 'NONE',  ( -15.45084971874736368, 46.40000000000000568, 47.55282581475768211 ) ) ;
#639 = CARTESIAN_POINT ( 'NONE',  ( 15.45084971874737789, 20.38125000068279746, 47.55282581475767500 ) ) ;
#640 = CARTESIAN_POINT ( 'NONE',  ( -17.50000000000000000, 22.50000000000000000, 80.00000000000000000 ) ) ;
#641 = ORIENTED_EDGE ( 'NONE', *, *, #12919, .T. ) ;
#642 =( GEOMETRIC_REPRESENTATION_CONTEXT ( 3 ) GLOBAL_UNCERTAINTY_ASSIGNED_CONTEXT ( ( #2937 ) ) GLOBAL_UNIT_ASSIGNED_CONTEXT ( ( #15209, #12566, #3759 ) ) REPRESENTATION_CONTEXT ( 'NONE', 'WORKASPACE' ) );
#643 = CARTESIAN_POINT ( 'NONE',  ( -40.34137639590981905, 31.65937500034139873, -29.30972558990011478 ) ) ;
#644 = ORIENTED_EDGE ( 'NONE', *, *, #6590, .T. ) ;
#645 = ORIENTED_EDGE ( 'NONE', *, *, #4809, .T. ) ;
#646 = VERTEX_POINT ( 'NONE', #3935 ) ;
#647 = CARTESIAN_POINT ( 'NONE',  ( -15.45084971874736368, 46.18125000068280173, 47.55282581475768211 ) ) ;
#648 = DIRECTION ( 'NONE',  ( 0.000000000000000000, 8.780190904559502465E-17, 1.000000000000000000 ) ) ;
#649 = CARTESIAN_POINT ( 'NONE',  ( -49.86468353125000164, 21.85937500034139802, 0.000000000000000000 ) ) ;
#650 = ORIENTED_EDGE ( 'NONE', *, *, #1309, .F. ) ;
#651 = CARTESIAN_POINT ( 'NONE',  ( -1.240322475938754499E-13, 38.50000000000000711, 50.00000000000000000 ) ) ;
#652 = CARTESIAN_POINT ( 'NONE',  ( -4.056709942754369358, 5.819547430268732668, 101.3333374614808662 ) ) ;
#653 = DIRECTION ( 'NONE',  ( 0.000000000000000000, 1.000000000000000000, 0.000000000000000000 ) ) ;
#654 = CYLINDRICAL_SURFACE ( 'NONE', #8851, 50.00000000000000000 ) ;
#655 = CARTESIAN_POINT ( 'NONE',  ( 9.631387414534489405E-15, 28.42187500034139447, 52.43083105670540789 ) ) ;
#657 = EDGE_CURVE ( 'NONE', #9775, #5127, #7632, .T. ) ;
#656 = AXIS2_PLACEMENT_3D ( 'NONE', #7217, #7053, #1959 ) ;
#658 = CARTESIAN_POINT ( 'NONE',  ( -40.45084971874737079, 32.20000000000000284, 29.38926261462367151 ) ) ;
#659 = ADVANCED_FACE ( 'NONE', ( #13818 ), #1344, .F. ) ;
#660 = DIRECTION ( 'NONE',  ( 0.000000000000000000, 0.000000000000000000, 1.000000000000000000 ) ) ;
#661 = STYLED_ITEM ( 'NONE', ( #15532 ), #11759 ) ;
#662 = FACE_OUTER_BOUND ( 'NONE', #4298, .T. ) ;
#663 = CARTESIAN_POINT ( 'NONE',  ( 49.86468353124999453, 23.02187500034139944, -16.20201782572376104 ) ) ;
#664 = DIRECTION ( 'NONE',  ( -0.9961946980917455452, 0.08715574274765797158, 0.000000000000000000 ) ) ;
#665 = CARTESIAN_POINT ( 'NONE',  ( -40.45084971874737789, 31.80000000000000071, -29.38926261462365730 ) ) ;
#666 = CARTESIAN_POINT ( 'NONE',  ( 40.34137639590981195, 29.05937500034139376, -29.30972558990011834 ) ) ;
#667 = ORIENTED_EDGE ( 'NONE', *, *, #5236, .F. ) ;
#668 = AXIS2_PLACEMENT_3D ( 'NONE', #6556, #5317, #14175 ) ;
#669 = CARTESIAN_POINT ( 'NONE',  ( -15.40903463028480580, 28.25937500034139660, 47.42413220539094709 ) ) ;
#670 = ORIENTED_EDGE ( 'NONE', *, *, #3372, .F. ) ;
#671 = COLOUR_RGB ( '', 0.09019608, 0.27058824, 0.51372549) ;
#672 = DIRECTION ( 'NONE',  ( 1.000000000000000000, 0.000000000000000000, -0.000000000000000000 ) ) ;
#673 = CARTESIAN_POINT ( 'NONE',  ( 30.81806926056962936, 39.15937500034139873, -42.41743335407647209 ) ) ;
#674 = B_SPLINE_CURVE_WITH_KNOTS ( 'NONE', 3,
 ( #4274, #1766, #9418, #9340 ),
 .UNSPECIFIED., .F., .F.,
 ( 4, 4 ),
 ( 2.829004760702349710E-07, 0.001414802801989369606 ),
 .UNSPECIFIED. ) ;
#675 = LINE ( 'NONE', #11094, #3539 ) ;
#676 = DIRECTION ( 'NONE',  ( 0.000000000000000000, 0.000000000000000000, -1.000000000000000000 ) ) ;
#677 = VECTOR ( 'NONE', #999, 1000.000000000000114 ) ;
#678 = CARTESIAN_POINT ( 'NONE',  ( 49.86468353125001585, 26.82187500034138949, 16.20201782572375038 ) ) ;
#679 = CARTESIAN_POINT ( 'NONE',  ( -49.86468353124999453, 33.95937500034139589, 16.20201782572377169 ) ) ;
#680 = VECTOR ( 'NONE', #908, 1000.000000000000000 ) ;
#681 = AXIS2_PLACEMENT_3D ( 'NONE', #11414, #6347, #2840 ) ;
#682 = CARTESIAN_POINT ( 'NONE',  ( -9.877534094663211306, 8.054089844915763408, 101.0000000000000000 ) ) ;
#683 = CARTESIAN_POINT ( 'NONE',  ( -40.34137639590981905, 27.72187500034139873, -29.30972558990011478 ) ) ;
#684 = CIRCLE ( 'NONE', #9999, 82.49773270518484480 ) ;
#685 = CIRCLE ( 'NONE', #1492, 47.00000000000000000 ) ;
#686 = CARTESIAN_POINT ( 'NONE',  ( 5.000000000000000000, 92.00000000000001421, 0.000000000000000000 ) ) ;
#687 = CARTESIAN_POINT ( 'NONE',  ( -49.86468353124999453, 45.75937500034140015, -16.20201782572375393 ) ) ;
#688 = CARTESIAN_POINT ( 'NONE',  ( -3.210462471511496205E-15, 43.42187500034140157, -52.43083105670540789 ) ) ;
#689 =( BOUNDED_CURVE ( )  B_SPLINE_CURVE ( 2, ( #16294, #2487, #7565, #8893, #2576, #11470, #15284, #2732, #3913, #1400, #7810, #4068, #13209 ),
 .UNSPECIFIED., .F., .T. ) 
 B_SPLINE_CURVE_WITH_KNOTS ( ( 3, 2, 2, 2, 2, 2, 3 ),
 ( 0.8166666666666666519, 0.8199999999999999512, 0.8266666666666666607, 0.8333333333333333703, 0.8399999999999999689, 0.8466666666666666785, 0.8500000000000000888 ),
 .UNSPECIFIED. ) 
 CURVE ( )  GEOMETRIC_REPRESENTATION_ITEM ( )  RATIONAL_B_SPLINE_CURVE ( ( 0.9755282581475768211, 0.9755282581475768211, 1.000000000000000000, 0.9510565162951535312, 1.000000000000000000, 0.9510565162951535312, 1.000000000000000000, 0.9510565162951535312, 1.000000000000000000, 0.9510565162951535312, 1.000000000000000000, 0.9755282581475763770, 0.9755282581475768211 ) ) 
 REPRESENTATION_ITEM ( '' )  );
#690 = CARTESIAN_POINT ( 'NONE',  ( 40.34137639590981905, 22.72187500034139518, 29.30972558990010768 ) ) ;
#691 = VERTEX_POINT ( 'NONE', #7507 ) ;
#692 = CARTESIAN_POINT ( 'NONE',  ( 30.81806926056964002, 48.55937500034139020, 42.41743335407646498 ) ) ;
#693 = VECTOR ( 'NONE', #7436, 1000.000000000000000 ) ;
#694 = EDGE_LOOP ( 'NONE', ( #5052, #10178, #10771, #9327 ) ) ;
#695 = EDGE_LOOP ( 'NONE', ( #7195, #10121, #1457 ) ) ;
#696 = CIRCLE ( 'NONE', #10012, 45.00000000000000000 ) ;
#697 = VECTOR ( 'NONE', #8943, 1000.000000000000000 ) ;
#699 = CARTESIAN_POINT ( 'NONE',  ( -30.90169943749473802, 28.08125000068280031, 42.53254041760200721 ) ) ;
#698 = AXIS2_PLACEMENT_3D ( 'NONE', #9570, #3238, #12296 ) ;
#700 = ORIENTED_EDGE ( 'NONE', *, *, #4864, .F. ) ;
#701 = EDGE_CURVE ( 'NONE', #14905, #2524, #8950, .T. ) ;
#702 = CARTESIAN_POINT ( 'NONE',  ( -4.127528389677584286, 5.486372832567261604, 101.0000000000000000 ) ) ;
#703 = CARTESIAN_POINT ( 'NONE',  ( -3.210462471511496205E-15, 43.42187500034140157, -52.43083105670540789 ) ) ;
#704 = CARTESIAN_POINT ( 'NONE',  ( 9.631387414534489405E-15, 46.42187500034139447, 52.43083105670540789 ) ) ;
#705 = DIRECTION ( 'NONE',  ( 1.000000000000000000, 0.000000000000000000, -0.000000000000000000 ) ) ;
#706 = VECTOR ( 'NONE', #3589, 1000.000000000000114 ) ;
#707 = VECTOR ( 'NONE', #13794, 1000.000000000000227 ) ;
#708 = CARTESIAN_POINT ( 'NONE',  ( 15.45084971874737789, 40.60000000000000142, 47.55282581475767500 ) ) ;
#709 = AXIS2_PLACEMENT_3D ( 'NONE', #5217, #3952, #9026 ) ;
#711 = EDGE_CURVE ( 'NONE', #14691, #4152, #10547, .T. ) ;
#710 = CIRCLE ( 'NONE', #11875, 50.00000000000000000 ) ;
#712 = CARTESIAN_POINT ( 'NONE',  ( -30.81806926056962226, 42.22187500034139163, 42.41743335407647919 ) ) ;
#713 = FACE_OUTER_BOUND ( 'NONE', #12733, .T. ) ;
#714 = EDGE_LOOP ( 'NONE', ( #14088, #8765 ) ) ;
#715 = CARTESIAN_POINT ( 'NONE',  ( -15.40903463028480580, 40.32187500034140015, 47.42413220539094709 ) ) ;
#716 = EDGE_CURVE ( 'NONE', #9033, #5335, #1883, .T. ) ;
#717 = ORIENTED_EDGE ( 'NONE', *, *, #6005, .F. ) ;
#718 = ORIENTED_EDGE ( 'NONE', *, *, #251, .F. ) ;
#719 = ORIENTED_EDGE ( 'NONE', *, *, #2125, .T. ) ;
#720 = FACE_OUTER_BOUND ( 'NONE', #12786, .T. ) ;
#721 = CARTESIAN_POINT ( 'NONE',  ( 0.000000000000000000, 272.0000000000000000, 0.000000000000000000 ) ) ;
#722 =( BOUNDED_CURVE ( )  B_SPLINE_CURVE ( 2, ( #13103, #13189, #11525, #15348, #2961, #2709, #1463, #9040, #11857, #15677, #292, #15427, #1708, #11770, #7789, #4222, #14094, #6468, #8029, #123, #9117, #2884, #6721, #9367, #14176, #2794, #7869, #3965, #6805, #1551, #4303, #9207, #14263, #459, #12858, #10368, #6644, #5391, #5238, #10294, #10542, #10450, #15506, #4132, #6557, #11617, #8109, #7953, #9289, #215, #13025, #1627, #14345, #5562, #5318, #370, #5473, #14417, #3037, #15601, #2112, #7125, #12096, #14741, #12015, #703, #11937, #2034, #538, #5791, #782, #4627, #6885, #9689, #9535, #5874, #1793, #3204, #863, #12262, #1866, #14829, #5632, #10936, #12183, #10696, #16000, #3376, #10858, #8441, #15924, #3286, #15752, #4546, #13505, #4380, #3458, #11020, #7039, #15844, #9609, #7199, #6962, #614, #13343, #14658, #8355, #5958, #16088, #5710, #13424, #9445, #4723, #14499, #9784, #8519, #3128, #8200, #1946, #13266, #10778, #4468, #14579, #8277, #14059, #1260, #1419, #4091, #10167, #945, #4012, #13584, #11489, #13889, #2753, #7671, #2191, #12663, #6351, #4806, #11417, #6429, #13976, #12904, #10246, #6044, #14138, #255, #5360, #9, #7829, #11115, #15217, #15307, #5112, #9082, #86, #1512, #10089, #5191, #12741, #10414, #16176, #6604, #6511, #11657, #7288, #15470, #2595, #12344, #7585, #15139, #3846, #3767, #8826, #3930, #9001, #2504, #176, #8912, #1339, #2675, #7749, #12817, #11568, #5281, #10332, #15390, #13306, #14305, #8072, #4344, #15641, #7000, #575, #11814, #4428, #10585, #1830, #5599, #11979, #1906, #2844, #11901, #10825, #8163, #6769, #6925, #12988, #1671, #3171, #9252, #11734, #9161, #4185, #655, #15797, #1592, #10737, #6686, #12055, #8240, #9497, #13145, #4264, #420, #5522, #5670, #336, #9331, #5756, #2927, #5435, #14218, #7994, #15888, #14543, #10497, #7911, #15555, #13068, #14382, #3003, #1754, #6853, #500, #9409, #10661, #15714, #14455, #3086 ),
 .UNSPECIFIED., .F., .T. ) 
 B_SPLINE_CURVE_WITH_KNOTS ( ( 3, 2, 2, 2, 2, 2, 2, 2, 2, 2, 2, 2, 2, 2, 2, 2, 2, 2, 2, 2, 2, 2, 2, 2, 2, 2, 2, 2, 2, 2, 2, 2, 2, 2, 2, 2, 2, 2, 2, 2, 2, 2, 2, 2, 2, 2, 2, 2, 2, 2, 2, 2, 2, 2, 2, 2, 2, 2, 2, 2, 2, 2, 2, 2, 2, 2, 2, 2, 2, 2, 2, 2, 2, 2, 2, 2, 2, 2, 2, 2, 2, 2, 2, 2, 2, 2, 2, 2, 2, 2, 2, 2, 2, 2, 2, 2, 2, 2, 2, 2, 2, 2, 2, 2, 2, 2, 2, 2, 2, 2, 2, 2, 2, 2, 2, 2, 2, 2, 2, 2, 2, 2, 2, 2, 2, 3 ),
 ( 0.000000000000000000, 0.006666666666666667095, 0.01333333333333333419, 0.02000000000000000042, 0.02666666666666666838, 0.03333333333333333287, 0.04000000000000000083, 0.04666666666666666879, 0.05333333333333333676, 0.05999999999999999778, 0.06666666666666666574, 0.07333333333333333370, 0.08000000000000000167, 0.08666666666666666963, 0.09333333333333333759, 0.1000000000000000194, 0.1066666666666666735, 0.1133333333333333276, 0.1199999999999999956, 0.1266666666666666774, 0.1333333333333333315, 0.1400000000000000133, 0.1466666666666666674, 0.1533333333333333215, 0.1600000000000000033, 0.1666666666666666574, 0.1733333333333333393, 0.1799999999999999933, 0.1866666666666666752, 0.1933333333333333570, 0.2000000000000000389, 0.2066666666666666652, 0.2133333333333333470, 0.2200000000000000011, 0.2266666666666666552, 0.2333333333333333370, 0.2399999999999999911, 0.2466666666666666730, 0.2533333333333333548, 0.2600000000000000089, 0.2666666666666666630, 0.2733333333333333171, 0.2800000000000000266, 0.2866666666666666807, 0.2933333333333333348, 0.2999999999999999889, 0.3066666666666666430, 0.3133333333333333526, 0.3200000000000000067, 0.3266666666666666052, 0.3333333333333333148, 0.3399999999999999689, 0.3466666666666666785, 0.3533333333333333326, 0.3599999999999999867, 0.3666666666666666408, 0.3733333333333333504, 0.3800000000000000044, 0.3866666666666667140, 0.3933333333333333126, 0.4000000000000000777, 0.4066666666666666763, 0.4133333333333333304, 0.4199999999999999845, 0.4266666666666666941, 0.4333333333333333481, 0.4400000000000000022, 0.4466666666666667118, 0.4533333333333333104, 0.4600000000000000755, 0.4666666666666666741, 0.4733333333333333282, 0.4799999999999999822, 0.4866666666666666918, 0.4933333333333333459, 0.5000000000000000000, 0.5066666666666667096, 0.5133333333333333082, 0.5200000000000000178, 0.5266666666666666163, 0.5333333333333333259, 0.5400000000000000355, 0.5466666666666666341, 0.5533333333333333437, 0.5600000000000000533, 0.5666666666666666519, 0.5733333333333333615, 0.5799999999999999600, 0.5866666666666666696, 0.5933333333333333792, 0.5999999999999999778, 0.6066666666666665764, 0.6133333333333332860, 0.6199999999999999956, 0.6266666666666667052, 0.6333333333333333037, 0.6400000000000000133, 0.6466666666666666119, 0.6533333333333332105, 0.6600000000000000311, 0.6666666666666666297, 0.6733333333333333393, 0.6799999999999999378, 0.6866666666666666474, 0.6933333333333333570, 0.6999999999999998446, 0.7066666666666666652, 0.7133333333333333748, 0.7199999999999999734, 0.7266666666666665719, 0.7333333333333332815, 0.7399999999999999911, 0.7466666666666667007, 0.7533333333333332993, 0.7600000000000000089, 0.7666666666666667185, 0.7733333333333334281, 0.7800000000000000266, 0.7866666666666666252, 0.7933333333333333348, 0.8000000000000001554, 0.8066666666666666430, 0.8133333333333333526, 0.8200000000000000622, 0.8266666666666666607, 0.8307121371438114243 ),
 .UNSPECIFIED. ) 
 CURVE ( )  GEOMETRIC_REPRESENTATION_ITEM ( )  RATIONAL_B_SPLINE_CURVE ( ( 1.000000000000000000, 0.9510565162951535312, 1.000000000000000000, 0.9510565162951535312, 1.000000000000000000, 0.9510565162951535312, 1.000000000000000000, 0.9510565162951535312, 1.000000000000000000, 0.9510565162951535312, 1.000000000000000000, 0.9510565162951535312, 1.000000000000000000, 0.9510565162951535312, 1.000000000000000000, 0.9510565162951535312, 1.000000000000000000, 0.9510565162951535312, 1.000000000000000000, 0.9510565162951535312, 1.000000000000000000, 0.9510565162951535312, 1.000000000000000000, 0.9510565162951535312, 1.000000000000000000, 0.9510565162951535312, 1.000000000000000000, 0.9510565162951535312, 1.000000000000000000, 0.9510565162951535312, 1.000000000000000000, 0.9510565162951535312, 1.000000000000000000, 0.9510565162951535312, 1.000000000000000000, 0.9510565162951535312, 1.000000000000000000, 0.9510565162951535312, 1.000000000000000000, 0.9510565162951535312, 1.000000000000000000, 0.9510565162951535312, 1.000000000000000000, 0.9510565162951535312, 1.000000000000000000, 0.9510565162951535312, 1.000000000000000000, 0.9510565162951535312, 1.000000000000000000, 0.9510565162951535312, 1.000000000000000000, 0.9510565162951535312, 1.000000000000000000, 0.9510565162951535312, 1.000000000000000000, 0.9510565162951535312, 1.000000000000000000, 0.9510565162951535312, 1.000000000000000000, 0.9510565162951535312, 1.000000000000000000, 0.9510565162951535312, 1.000000000000000000, 0.9510565162951535312, 1.000000000000000000, 0.9510565162951535312, 1.000000000000000000, 0.9510565162951535312, 1.000000000000000000, 0.9510565162951535312, 1.000000000000000000, 0.9510565162951535312, 1.000000000000000000, 0.9510565162951535312, 1.000000000000000000, 0.9510565162951535312, 1.000000000000000000, 0.9510565162951535312, 1.000000000000000000, 0.9510565162951535312, 1.000000000000000000, 0.9510565162951535312, 1.000000000000000000, 0.9510565162951535312, 1.000000000000000000, 0.9510565162951535312, 1.000000000000000000, 0.9510565162951535312, 1.000000000000000000, 0.9510565162951535312, 1.000000000000000000, 0.9510565162951535312, 1.000000000000000000, 0.9510565162951535312, 1.000000000000000000, 0.9510565162951535312, 1.000000000000000000, 0.9510565162951535312, 1.000000000000000000, 0.9510565162951535312, 1.000000000000000000, 0.9510565162951535312, 1.000000000000000000, 0.9510565162951535312, 1.000000000000000000, 0.9510565162951535312, 1.000000000000000000, 0.9510565162951535312, 1.000000000000000000, 0.9510565162951535312, 1.000000000000000000, 0.9510565162951535312, 1.000000000000000000, 0.9510565162951535312, 1.000000000000000000, 0.9510565162951535312, 1.000000000000000000, 0.9510565162951535312, 1.000000000000000000, 0.9510565162951535312, 1.000000000000000000, 0.9510565162951535312, 1.000000000000000000, 0.9510565162951535312, 1.000000000000000000, 0.9510565162951535312, 1.000000000000000000, 0.9510565162951535312, 1.000000000000000000, 0.9510565162951535312, 1.000000000000000000, 0.9510565162951535312, 1.000000000000000000, 0.9510565162951535312, 1.000000000000000000, 0.9510565162951535312, 1.000000000000000000, 0.9510565162951535312, 1.000000000000000000, 0.9510565162951535312, 1.000000000000000000, 0.9510565162951535312, 1.000000000000000000, 0.9510565162951535312, 1.000000000000000000, 0.9510565162951535312, 1.000000000000000000, 0.9510565162951535312, 1.000000000000000000, 0.9510565162951535312, 1.000000000000000000, 0.9510565162951535312, 1.000000000000000000, 0.9510565162951535312, 1.000000000000000000, 0.9510565162951535312, 1.000000000000000000, 0.9510565162951535312, 1.000000000000000000, 0.9510565162951535312, 1.000000000000000000, 0.9510565162951535312, 1.000000000000000000, 0.9510565162951535312, 1.000000000000000000, 0.9510565162951535312, 1.000000000000000000, 0.9510565162951535312, 1.000000000000000000, 0.9510565162951535312, 1.000000000000000000, 0.9510565162951535312, 1.000000000000000000, 0.9510565162951535312, 1.000000000000000000, 0.9510565162951535312, 1.000000000000000000, 0.9510565162951535312, 1.000000000000000000, 0.9510565162951535312, 1.000000000000000000, 0.9510565162951535312, 1.000000000000000000, 0.9510565162951535312, 1.000000000000000000, 0.9510565162951535312, 1.000000000000000000, 0.9510565162951535312, 1.000000000000000000, 0.9510565162951535312, 1.000000000000000000, 0.9510565162951535312, 1.000000000000000000, 0.9510565162951535312, 1.000000000000000000, 0.9510565162951535312, 1.000000000000000000, 0.9510565162951535312, 1.000000000000000000, 0.9510565162951535312, 1.000000000000000000, 0.9510565162951535312, 1.000000000000000000, 0.9510565162951535312, 1.000000000000000000, 0.9510565162951535312, 1.000000000000000000, 0.9510565162951535312, 1.000000000000000000, 0.9510565162951535312, 1.000000000000000000, 0.9510565162951535312, 1.000000000000000000, 0.9510565162951535312, 1.000000000000000000, 0.9510565162951535312, 1.000000000000000000, 0.9510565162951535312, 1.000000000000000000, 0.9510565162951535312, 1.000000000000000000, 0.9510565162951535312, 1.000000000000000000, 0.9510565162951535312, 1.000000000000000000, 0.9510565162951535312, 1.000000000000000000, 0.9510565162951535312, 1.000000000000000000, 0.9510565162951535312, 1.000000000000000000, 0.9510565162951535312, 1.000000000000000000, 0.9510565162951535312, 1.000000000000000000, 0.9510565162951535312, 1.000000000000000000, 0.9510565162951535312, 1.000000000000000000, 0.9510565162951535312, 1.000000000000000000, 0.9510565162951535312, 1.000000000000000000, 0.9510565162951535312, 1.000000000000000000, 0.9510565162951535312, 1.000000000000000000, 0.9510565162951535312, 1.000000000000000000, 0.9703000872435151303, 0.9766452105560694541 ) ) 
 REPRESENTATION_ITEM ( '' )  );
#723 = ADVANCED_FACE ( 'NONE', ( #12824 ), #12909, .T. ) ;
#724 = CARTESIAN_POINT ( 'NONE',  ( -4.126043002969710827, 5.493361027597350343, 101.0000000000000000 ) ) ;
#725 = CARTESIAN_POINT ( 'NONE',  ( 1.293669679204937499E-13, 37.50000000000000711, -50.00000000000000000 ) ) ;
#726 = CARTESIAN_POINT ( 'NONE',  ( 49.86468353125000164, 36.85937500034139447, -6.106662507704105588E-15 ) ) ;
#727 = CARTESIAN_POINT ( 'NONE',  ( -49.86468353124999453, 45.95937500034138878, 16.20201782572377169 ) ) ;
#728 = CARTESIAN_POINT ( 'NONE',  ( 0.000000000000000000, 282.0000000000000000, 0.000000000000000000 ) ) ;
#729 = DIRECTION ( 'NONE',  ( -0.000000000000000000, -0.000000000000000000, 1.000000000000000000 ) ) ;
#730 = SHAPE_REPRESENTATION_RELATIONSHIP ( 'NONE' , 'NONE' ,  #15829, #9194 ) ;
#731 = CARTESIAN_POINT ( 'NONE',  ( 6.661118525004998681, 38.69041383028350367, 102.0000000000000142 ) ) ;
#732 = CARTESIAN_POINT ( 'NONE',  ( -40.45084971874737079, 35.98125000068279888, 29.38926261462367151 ) ) ;
#733 = CIRCLE ( 'NONE', #6335, 9.080892972013911546 ) ;
#734 = FACE_OUTER_BOUND ( 'NONE', #14301, .T. ) ;
#735 = DIRECTION ( 'NONE',  ( 0.000000000000000000, 0.000000000000000000, 1.000000000000000000 ) ) ;
#736 = EDGE_LOOP ( 'NONE', ( #3284, #6956, #2417, #3297 ) ) ;
#737 = CARTESIAN_POINT ( 'NONE',  ( -30.81806926056962226, 28.15937500034139518, 42.41743335407647919 ) ) ;
#738 = ORIENTED_EDGE ( 'NONE', *, *, #13518, .F. ) ;
#739 = ORIENTED_EDGE ( 'NONE', *, *, #10784, .T. ) ;
#740 = ORIENTED_EDGE ( 'NONE', *, *, #6886, .T. ) ;
#741 = CARTESIAN_POINT ( 'NONE',  ( -40.45084971874737079, 43.98125000068279888, 29.38926261462367151 ) ) ;
#742 = LINE ( 'NONE', #7236, #3369 ) ;
#743 = CARTESIAN_POINT ( 'NONE',  ( 15.45084971874736723, 29.40000000000000213, -47.55282581475768211 ) ) ;
#744 = ORIENTED_EDGE ( 'NONE', *, *, #13835, .F. ) ;
#745 = CARTESIAN_POINT ( 'NONE',  ( 1.293669679204937499E-13, 37.50000000000000711, -50.00000000000000000 ) ) ;
#746 = CARTESIAN_POINT ( 'NONE',  ( -30.90169943749473447, 38.29999999999999716, 42.53254041760200721 ) ) ;
#747 = CARTESIAN_POINT ( 'NONE',  ( -49.99999999999999289, 20.09999999999999787, 16.24598481164533226 ) ) ;
#748 = DIRECTION ( 'NONE',  ( 0.000000000000000000, -1.000000000000000000, 0.000000000000000000 ) ) ;
#749 = DIRECTION ( 'NONE',  ( 0.000000000000000000, -0.000000000000000000, 1.000000000000000000 ) ) ;
#750 = DIRECTION ( 'NONE',  ( 0.000000000000000000, 1.000000000000000000, 0.000000000000000000 ) ) ;
#751 = CARTESIAN_POINT ( 'NONE',  ( -48.98979485566356828, 261.9999999999999432, -9.999999999999994671 ) ) ;
#752 = CARTESIAN_POINT ( 'NONE',  ( -43.39327851764683430, 20.00000000000000711, 25.00490296284258918 ) ) ;
#753 = CARTESIAN_POINT ( 'NONE',  ( -15.40903463028480580, 20.32187500034139660, 47.42413220539094709 ) ) ;
#754 = CARTESIAN_POINT ( 'NONE',  ( 9.657523855033129090E-15, 28.49999999999999645, 52.57311121191334990 ) ) ;
#755 = CARTESIAN_POINT ( 'NONE',  ( -15.40903463028481646, 23.45937500034139944, -47.42413220539093999 ) ) ;
#756 = CARTESIAN_POINT ( 'NONE',  ( 30.81806926056962936, 49.15937500034138452, -42.41743335407647209 ) ) ;
#757 = VECTOR ( 'NONE', #2822, 1000.000000000000000 ) ;
#758 = VERTEX_POINT ( 'NONE', #14387 ) ;
#759 = DIRECTION ( 'NONE',  ( 0.9361168066628589024, 0.08189960831908940642, 0.3420201433256691570 ) ) ;
#760 = EDGE_CURVE ( 'NONE', #1819, #7317, #14134, .T. ) ;
#761 = VERTEX_POINT ( 'NONE', #6932 ) ;
#762 = CARTESIAN_POINT ( 'NONE',  ( 40.45084971874737789, 48.80000000000000426, 29.38926261462365375 ) ) ;
#763 = CARTESIAN_POINT ( 'NONE',  ( -49.86468353124999453, 35.95937500034139589, 16.20201782572377525 ) ) ;
#764 = CARTESIAN_POINT ( 'NONE',  ( 50.00000000000000711, 48.68125000068279462, 16.24598481164530739 ) ) ;
#765 = CARTESIAN_POINT ( 'NONE',  ( -3.111920190527341144E-15, 45.28125000068279604, -50.00000000000000000 ) ) ;
#766 = PRESENTATION_LAYER_ASSIGNMENT (  '', '', ( #7431 ) ) ;
#767 = CARTESIAN_POINT ( 'NONE',  ( -49.86468353124999453, 29.82187500034139660, -16.20201782572375393 ) ) ;
#768 = CARTESIAN_POINT ( 'NONE',  ( 30.81806926056964002, 32.55937500034139731, 42.41743335407646498 ) ) ;
#769 = CARTESIAN_POINT ( 'NONE',  ( 0.000000000000000000, 22.50000000000000000, 101.0000000000000000 ) ) ;
#770 = CARTESIAN_POINT ( 'NONE',  ( -30.81806926056963292, 29.62187500034139376, -42.41743335407647209 ) ) ;
#771 = CARTESIAN_POINT ( 'NONE',  ( 49.99999999999999289, 33.10000000000000142, -16.24598481164532160 ) ) ;
#772 = CARTESIAN_POINT ( 'NONE',  ( 9.631387414534489405E-15, 46.35937500034139447, 52.43083105670540789 ) ) ;
#773 = CARTESIAN_POINT ( 'NONE',  ( 30.81806926056962936, 35.22187500034138452, -42.41743335407647209 ) ) ;
#774 = CARTESIAN_POINT ( 'NONE',  ( 9.631387414534489405E-15, 22.42187500034139802, 52.43083105670540789 ) ) ;
#775 = ORIENTED_EDGE ( 'NONE', *, *, #10887, .F. ) ;
#776 = MECHANICAL_DESIGN_GEOMETRIC_PRESENTATION_REPRESENTATION (  '', ( #10358 ), #14324 ) ;
#777 = CARTESIAN_POINT ( 'NONE',  ( -49.86468353124999453, 41.95937500034139589, 16.20201782572377169 ) ) ;
#778 = ORIENTED_EDGE ( 'NONE', *, *, #1765, .T. ) ;
#779 = CARTESIAN_POINT ( 'NONE',  ( -49.99999999999999289, 33.68125000068278752, -16.24598481164531449 ) ) ;
#780 = ORIENTED_EDGE ( 'NONE', *, *, #7914, .F. ) ;
#781 = CARTESIAN_POINT ( 'NONE',  ( -7.919222016226688865, 33.33250428222964956, -50.00000000000003553 ) ) ;
#782 = CARTESIAN_POINT ( 'NONE',  ( 49.86468353125000164, 42.92187500034140157, -6.106662507704105588E-15 ) ) ;
#783 = CARTESIAN_POINT ( 'NONE',  ( -49.86468353124999453, 19.95937500034138878, 16.20201782572377525 ) ) ;
#784 = CARTESIAN_POINT ( 'NONE',  ( 9.642970592016636644, 101.1563493904846780, 1.872989114519530984 ) ) ;
#785 = ADVANCED_FACE ( 'NONE', ( #11984 ), #5440, .T. ) ;
#786 = CARTESIAN_POINT ( 'NONE',  ( -15.40903463028480580, 22.32187500034139660, 47.42413220539094709 ) ) ;
#787 = EDGE_CURVE ( 'NONE', #4002, #5069, #14947, .T. ) ;
#788 = PRODUCT_CONTEXT ( 'NONE', #6541, 'mechanical' ) ;
#789 = CARTESIAN_POINT ( 'NONE',  ( -40.45084971874737079, 31.98125000068280244, 29.38926261462367151 ) ) ;
#790 = CARTESIAN_POINT ( 'NONE',  ( -50.00000000000000000, 36.00000000000000711, 0.000000000000000000 ) ) ;
#791 = CARTESIAN_POINT ( 'NONE',  ( 15.40903463028481113, 43.32187500034139305, -47.42413220539094709 ) ) ;
#792 = LINE ( 'NONE', #5882, #7783 ) ;
#793 = VERTEX_POINT ( 'NONE', #6609 ) ;
#794 = EDGE_CURVE ( 'NONE', #9739, #6366, #6691, .T. ) ;
#795 = CARTESIAN_POINT ( 'NONE',  ( 30.81806926056962936, 43.22187500034140584, -42.41743335407647209 ) ) ;
#796 = DIRECTION ( 'NONE',  ( -1.000000000000000000, 0.000000000000000000, -0.000000000000000000 ) ) ;
#797 = ORIENTED_EDGE ( 'NONE', *, *, #14711, .F. ) ;
#798 = VERTEX_POINT ( 'NONE', #9337 ) ;
#799 = ORIENTED_EDGE ( 'NONE', *, *, #441, .T. ) ;
#800 = EDGE_CURVE ( 'NONE', #6081, #8593, #7999, .T. ) ;
#801 = CARTESIAN_POINT ( 'NONE',  ( 7.960204194457797252E-15, 52.00000000000000711, -65.00000000000000000 ) ) ;
#802 = DIRECTION ( 'NONE',  ( 0.000000000000000000, 0.000000000000000000, 1.000000000000000000 ) ) ;
#803 = CARTESIAN_POINT ( 'NONE',  ( -2.547328955960238000E-13, 22.28125000068279604, 49.99999999999999289 ) ) ;
#804 = CARTESIAN_POINT ( 'NONE',  ( 49.99999999999999289, 36.88125000068279036, -16.24598481164532160 ) ) ;
#805 = CARTESIAN_POINT ( 'NONE',  ( -30.81806926056962226, 38.15937500034138452, 42.41743335407647919 ) ) ;
#806 = CARTESIAN_POINT ( 'NONE',  ( -40.34137639590981905, 45.65937500034139873, -29.30972558990011478 ) ) ;
#807 = CARTESIAN_POINT ( 'NONE',  ( 30.90169943749473802, 25.30000000000000071, -42.53254041760200721 ) ) ;
#808 = CARTESIAN_POINT ( 'NONE',  ( 6.123233995736766085E-15, 193.4213562373095385, 50.00000000000000000 ) ) ;
#809 =( NAMED_UNIT ( * ) PLANE_ANGLE_UNIT ( ) SI_UNIT ( $, .RADIAN. ) );
#810 = CARTESIAN_POINT ( 'NONE',  ( 9.297345850538470396E-15, 92.00000000000001421, -1.969248798088869855E-14 ) ) ;
#811 = CARTESIAN_POINT ( 'NONE',  ( 0.000000000000000000, 193.4213562373095385, -50.00000000000000000 ) ) ;
#812 = CARTESIAN_POINT ( 'NONE',  ( 30.90169943749475223, 42.48125000068279888, 42.53254041760199300 ) ) ;
#813 = LINE ( 'NONE', #10649, #1917 ) ;
#814 = ORIENTED_EDGE ( 'NONE', *, *, #8434, .F. ) ;
#815 = EDGE_CURVE ( 'NONE', #11124, #14188, #16130, .T. ) ;
#816 = CARTESIAN_POINT ( 'NONE',  ( 30.81806926056964002, 32.55937500034139731, 42.41743335407647209 ) ) ;
#817 = EDGE_LOOP ( 'NONE', ( #2895, #1858, #470, #5587, #7961 ) ) ;
#818 = ORIENTED_EDGE ( 'NONE', *, *, #5743, .T. ) ;
#819 = ORIENTED_EDGE ( 'NONE', *, *, #13945, .T. ) ;
#820 =( BOUNDED_CURVE ( )  B_SPLINE_CURVE ( 2, ( #15392, #6687, #13234, #3087, #10333, #5524, #4346, #4266, #15642, #14383, #1832, #13070, #9332 ),
 .UNSPECIFIED., .F., .F. ) 
 B_SPLINE_CURVE_WITH_KNOTS ( ( 3, 2, 2, 2, 2, 2, 3 ),
 ( 0.3833333333333333592, 0.3866666666666666585, 0.3933333333333333126, 0.4000000000000000222, 0.4066666666666666763, 0.4133333333333333304, 0.4166666666666666852 ),
 .UNSPECIFIED. ) 
 CURVE ( )  GEOMETRIC_REPRESENTATION_ITEM ( )  RATIONAL_B_SPLINE_CURVE ( ( 0.9755282581475768211, 0.9755282581475770431, 1.000000000000000000, 0.9510565162951535312, 1.000000000000000000, 0.9510565162951535312, 1.000000000000000000, 0.9510565162951535312, 1.000000000000000000, 0.9510565162951535312, 1.000000000000000000, 0.9755282581475765991, 0.9755282581475768211 ) ) 
 REPRESENTATION_ITEM ( '' )  );
#821 = CARTESIAN_POINT ( 'NONE',  ( 40.45084971874737079, 42.98125000068279888, -29.38926261462366440 ) ) ;
#822 = CARTESIAN_POINT ( 'NONE',  ( -15.45084971874737256, 39.60000000000000142, -47.55282581475767500 ) ) ;
#823 = CARTESIAN_POINT ( 'NONE',  ( 6.123233995736766085E-15, 20.00000000000000355, -50.00000000000000000 ) ) ;
#824 = ORIENTED_EDGE ( 'NONE', *, *, #7579, .T. ) ;
#825 = LINE ( 'NONE', #16289, #14432 ) ;
#826 = EDGE_CURVE ( 'NONE', #11404, #10795, #164, .T. ) ;
#827 = DIRECTION ( 'NONE',  ( 1.734723475976807094E-17, 0.000000000000000000, -1.000000000000000000 ) ) ;
#828 = DIRECTION ( 'NONE',  ( 1.000000000000000000, -5.352861011585576290E-15, 0.000000000000000000 ) ) ;
#829 = CARTESIAN_POINT ( 'NONE',  ( -49.93234176562499727, 49.96093750017070079, 0.000000000000000000 ) ) ;
#830 = DIRECTION ( 'NONE',  ( -0.000000000000000000, -0.000000000000000000, 1.000000000000000000 ) ) ;
#831 = CARTESIAN_POINT ( 'NONE',  ( -30.90169943749474513, 47.70000000000000284, -42.53254041760200721 ) ) ;
#832 = EDGE_CURVE ( 'NONE', #2646, #12589, #15834, .T. ) ;
#833 = LINE ( 'NONE', #15967, #10244 ) ;
#834 = CARTESIAN_POINT ( 'NONE',  ( -45.40153297753673201, 20.00000000000001776, 20.62078143446483480 ) ) ;
#835 = CARTESIAN_POINT ( 'NONE',  ( 49.86468353125000164, 24.92187500034139802, -6.106662507704105588E-15 ) ) ;
#836 = CARTESIAN_POINT ( 'NONE',  ( 0.000000000000000000, 22.50000000000000000, 80.00000000000000000 ) ) ;
#837 = CARTESIAN_POINT ( 'NONE',  ( -49.99999999999999289, 25.89999999999999858, -16.24598481164531449 ) ) ;
#838 = CARTESIAN_POINT ( 'NONE',  ( -49.86468353124999453, 27.95937500034139944, 16.20201782572377525 ) ) ;
#839 = CARTESIAN_POINT ( 'NONE',  ( -49.86468353124999453, 47.95937500034138878, 16.20201782572377525 ) ) ;
#840 = ORIENTED_EDGE ( 'NONE', *, *, #2746, .T. ) ;
#841 = CARTESIAN_POINT ( 'NONE',  ( 30.90169943749475223, 44.69999999999999574, 42.53254041760199300 ) ) ;
#842 = VERTEX_POINT ( 'NONE', #9257 ) ;
#843 = CARTESIAN_POINT ( 'NONE',  ( 0.000000000000000000, 267.0000000000000000, 0.000000000000000000 ) ) ;
#844 = CARTESIAN_POINT ( 'NONE',  ( 30.81806926056962936, 35.15937500034139873, -42.41743335407647209 ) ) ;
#845 = DIRECTION ( 'NONE',  ( -0.9135454576426004225, -0.4067366430758009854, 0.000000000000000000 ) ) ;
#846 = ADVANCED_FACE ( 'NONE', ( #581, #11664 ), #5365, .T. ) ;
#847 = FACE_OUTER_BOUND ( 'NONE', #8952, .T. ) ;
#848 = DIRECTION ( 'NONE',  ( 0.000000000000000000, 0.000000000000000000, 1.000000000000000000 ) ) ;
#849 = CARTESIAN_POINT ( 'NONE',  ( -15.40903463028480580, 32.32187500034139305, 47.42413220539094709 ) ) ;
#850 = CARTESIAN_POINT ( 'NONE',  ( 40.34137639590981905, 30.65937500034139518, 29.30972558990010768 ) ) ;
#851 = CARTESIAN_POINT ( 'NONE',  ( 0.000000000000000000, 247.0000000000000284, 0.000000000000000000 ) ) ;
#852 = CARTESIAN_POINT ( 'NONE',  ( 15.40903463028481113, 33.32187500034139305, -47.42413220539094709 ) ) ;
#853 = DIRECTION ( 'NONE',  ( 0.000000000000000000, 0.7071067811865487940, 0.7071067811865463515 ) ) ;
#854 = CARTESIAN_POINT ( 'NONE',  ( 49.86468353125001585, 46.75937500034140015, 16.20201782572375038 ) ) ;
#855 = CARTESIAN_POINT ( 'NONE',  ( 9.631387414534489405E-15, 40.42187500034138736, 52.43083105670540789 ) ) ;
#856 = AXIS2_PLACEMENT_3D ( 'NONE', #7471, #15025, #3813 ) ;
#857 = CARTESIAN_POINT ( 'NONE',  ( 15.40903463028482356, 24.52187500034139589, 47.42413220539093999 ) ) ;
#858 = ORIENTED_EDGE ( 'NONE', *, *, #1166, .T. ) ;
#859 = CARTESIAN_POINT ( 'NONE',  ( 49.86468353124999453, 42.95937500034139589, -16.20201782572376104 ) ) ;
#860 = VERTEX_POINT ( 'NONE', #11908 ) ;
#861 = CARTESIAN_POINT ( 'NONE',  ( 30.90169943749475578, 22.48125000068279533, 42.53254041760200010 ) ) ;
#862 = ORIENTED_EDGE ( 'NONE', *, *, #15437, .F. ) ;
#863 = CARTESIAN_POINT ( 'NONE',  ( -40.34137639590981195, 42.12187500034139731, 29.30972558990012189 ) ) ;
#864 = CARTESIAN_POINT ( 'NONE',  ( -40.34137639590981905, 21.65937500034139518, -29.30972558990011478 ) ) ;
#865 = CARTESIAN_POINT ( 'NONE',  ( 15.45084971874736723, 41.40000000000000568, -47.55282581475768211 ) ) ;
#866 = CARTESIAN_POINT ( 'NONE',  ( -49.86468353125000164, 25.92187500034139802, 0.000000000000000000 ) ) ;
#867 = ITEM_DEFINED_TRANSFORMATION ( 'NONE', 'NONE', #10797,  #15812 ) ;
#868 = CARTESIAN_POINT ( 'NONE',  ( -49.99999999999999289, 31.88125000068280102, 16.24598481164533226 ) ) ;
#869 = CARTESIAN_POINT ( 'NONE',  ( 40.34137639590981195, 41.12187500034139731, -29.30972558990011834 ) ) ;
#870 = CARTESIAN_POINT ( 'NONE',  ( -26.23306594130729863, 283.6958662468272792, -4.966131882590582691 ) ) ;
#871 = VERTEX_POINT ( 'NONE', #4096 ) ;
#872 = TOROIDAL_SURFACE ( 'NONE', #3283, 88.87749532708107836, 2.000000000000000000 ) ;
#873 = CARTESIAN_POINT ( 'NONE',  ( 40.34137639590981195, 37.12187500034139731, -29.30972558990011834 ) ) ;
#874 = CARTESIAN_POINT ( 'NONE',  ( 3.407225380398686276, 31.38205016914263723, 102.0000000000000142 ) ) ;
#875 = ORIENTED_EDGE ( 'NONE', *, *, #8946, .T. ) ;
#876 = ORIENTED_EDGE ( 'NONE', *, *, #11887, .F. ) ;
#877 = ORIENTED_EDGE ( 'NONE', *, *, #7745, .T. ) ;
#878 = DIRECTION ( 'NONE',  ( 0.8660254037844363761, 0.5000000000000041078, 0.000000000000000000 ) ) ;
#879 = LINE ( 'NONE', #9875, #7578 ) ;
#880 = CARTESIAN_POINT ( 'NONE',  ( -15.45084971874737256, 49.38125000068280457, -47.55282581475767500 ) ) ;
#881 = LINE ( 'NONE', #9625, #1539 ) ;
#882 = CARTESIAN_POINT ( 'NONE',  ( -49.86468353124999453, 35.75937500034140015, -16.20201782572375393 ) ) ;
#883 = CARTESIAN_POINT ( 'NONE',  ( -3.210462471511496205E-15, 49.35937500034138736, -52.43083105670540789 ) ) ;
#884 = CARTESIAN_POINT ( 'NONE',  ( 50.00000000000000711, 24.89999999999999858, 16.24598481164530739 ) ) ;
#885 = CIRCLE ( 'NONE', #362, 10.00000000000000000 ) ;
#886 = CARTESIAN_POINT ( 'NONE',  ( -2.547328955960238000E-13, 30.49999999999999645, 49.99999999999999289 ) ) ;
#887 = CARTESIAN_POINT ( 'NONE',  ( 30.00000000000000000, 282.0000000000000000, 12.50000000000000178 ) ) ;
#888 = CARTESIAN_POINT ( 'NONE',  ( -6.661118525005218949, 38.69041383028340420, 102.0000000000000142 ) ) ;
#889 = DIRECTION ( 'NONE',  ( -0.000000000000000000, -0.000000000000000000, 1.000000000000000000 ) ) ;
#890 = DIRECTION ( 'NONE',  ( 0.000000000000000000, 0.000000000000000000, -1.000000000000000000 ) ) ;
#891 = VERTEX_POINT ( 'NONE', #12993 ) ;
#892 = CARTESIAN_POINT ( 'NONE',  ( -30.81806926056963292, 31.55937500034139731, -42.41743335407647209 ) ) ;
#893 = ORIENTED_EDGE ( 'NONE', *, *, #4265, .F. ) ;
#894 = VERTEX_POINT ( 'NONE', #14312 ) ;
#895 = VERTEX_POINT ( 'NONE', #1676 ) ;
#896 = AXIS2_PLACEMENT_3D ( 'NONE', #7779, #2786, #3798 ) ;
#897 = CARTESIAN_POINT ( 'NONE',  ( -40.45084971874737789, 41.58125000068280031, -29.38926261462365730 ) ) ;
#898 = FACE_OUTER_BOUND ( 'NONE', #2362, .T. ) ;
#899 = DIRECTION ( 'NONE',  ( -1.000000000000000000, 0.000000000000000000, -0.000000000000000000 ) ) ;
#900 = ORIENTED_EDGE ( 'NONE', *, *, #11699, .F. ) ;
#901 = CARTESIAN_POINT ( 'NONE',  ( 2.978552182361884590E-14, 47.28125000068279604, -50.00000000000000000 ) ) ;
#902 = CARTESIAN_POINT ( 'NONE',  ( -2.168404344971008868E-16, 282.0000000000000000, 12.50000000000000000 ) ) ;
#903 = CARTESIAN_POINT ( 'NONE',  ( -16.94192497067215797, 17.96950525308796287, 95.33822655640803134 ) ) ;
#904 = CARTESIAN_POINT ( 'NONE',  ( 2.600676159226421000E-13, 21.28125000068279604, -49.99999999999999289 ) ) ;
#905 = CARTESIAN_POINT ( 'NONE',  ( -2.445080149700054274E-14, 46.28125000068280315, 50.00000000000000000 ) ) ;
#906 = CARTESIAN_POINT ( 'NONE',  ( 8.660254037844387298, 28.00000000000000355, 5.000000000000000000 ) ) ;
#907 = ADVANCED_FACE ( 'NONE', ( #507 ), #6097, .T. ) ;
#908 = DIRECTION ( 'NONE',  ( 0.5000000000000103251, 0.000000000000000000, 0.8660254037844327124 ) ) ;
#909 = CARTESIAN_POINT ( 'NONE',  ( 0.000000000000000000, 262.0000000000000000, 79.49773270518484480 ) ) ;
#910 = CARTESIAN_POINT ( 'NONE',  ( -50.00000000000000000, 47.78125000068279604, 0.000000000000000000 ) ) ;
#911 = CYLINDRICAL_SURFACE ( 'NONE', #979, 50.00000000000000000 ) ;
#912 = CARTESIAN_POINT ( 'NONE',  ( 30.90169943749475578, 26.70000000000000284, 42.53254041760200010 ) ) ;
#913 = CARTESIAN_POINT ( 'NONE',  ( -40.34137639590981195, 28.05937500034139731, 29.30972558990012189 ) ) ;
#914 = CARTESIAN_POINT ( 'NONE',  ( -40.45084971874737079, 44.20000000000000284, 29.38926261462367151 ) ) ;
#915 = EDGE_CURVE ( 'NONE', #9440, #646, #6307, .T. ) ;
#916 = ADVANCED_FACE ( 'NONE', ( #11164 ), #4772, .F. ) ;
#917 = DIRECTION ( 'NONE',  ( 1.000000000000000000, 0.000000000000000000, 0.000000000000000000 ) ) ;
#918 = ORIENTED_EDGE ( 'NONE', *, *, #1112, .T. ) ;
#919 = DIRECTION ( 'NONE',  ( -0.000000000000000000, 0.000000000000000000, 1.000000000000000000 ) ) ;
#920 = EDGE_LOOP ( 'NONE', ( #2916, #8700, #11462, #7137 ) ) ;
#921 = DIRECTION ( 'NONE',  ( 0.9361168066628589024, 0.08189960831908940642, 0.3420201433256691015 ) ) ;
#922 = CARTESIAN_POINT ( 'NONE',  ( -30.81806926056963292, 37.55937500034139020, -42.41743335407647209 ) ) ;
#923 = VECTOR ( 'NONE', #11786, 1000.000000000000000 ) ;
#924 = CARTESIAN_POINT ( 'NONE',  ( 0.000000000000000000, 193.4213562373095385, -50.00000000000000000 ) ) ;
#925 = DIRECTION ( 'NONE',  ( -0.000000000000000000, -0.000000000000000000, -1.000000000000000000 ) ) ;
#926 = LINE ( 'NONE', #8666, #14148 ) ;
#927 = DIRECTION ( 'NONE',  ( 0.000000000000000000, 0.000000000000000000, 1.000000000000000000 ) ) ;
#928 = CARTESIAN_POINT ( 'NONE',  ( -49.86468353124999453, 27.82187500034139305, -16.20201782572375393 ) ) ;
#929 = CARTESIAN_POINT ( 'NONE',  ( -30.81806926056962226, 32.15937500034139873, 42.41743335407647209 ) ) ;
#930 = DIRECTION ( 'NONE',  ( 0.000000000000000000, -1.000000000000000000, 0.000000000000000000 ) ) ;
#931 = CARTESIAN_POINT ( 'NONE',  ( -30.81806926056963292, 31.62187500034139731, -42.41743335407647209 ) ) ;
#932 = CARTESIAN_POINT ( 'NONE',  ( 15.45084971874737789, 32.60000000000000142, 47.55282581475767500 ) ) ;
#933 = CARTESIAN_POINT ( 'NONE',  ( 49.86468353125000164, 44.85937500034140157, -6.106662507704105588E-15 ) ) ;
#934 = CARTESIAN_POINT ( 'NONE',  ( -49.86468353124999453, 39.82187500034140015, -16.20201782572375393 ) ) ;
#935 = AXIS2_PLACEMENT_3D ( 'NONE', #14011, #3725, #13846 ) ;
#936 = CARTESIAN_POINT ( 'NONE',  ( -3.219174618344376363E-15, 49.50000000000000711, -52.57311121191334990 ) ) ;
#937 = ORIENTED_EDGE ( 'NONE', *, *, #15743, .F. ) ;
#938 = CARTESIAN_POINT ( 'NONE',  ( -49.86468353124999453, 43.95937500034138878, 16.20201782572377169 ) ) ;
#939 = ORIENTED_EDGE ( 'NONE', *, *, #11943, .F. ) ;
#940 = CARTESIAN_POINT ( 'NONE',  ( -30.90169943749474868, 27.48125000068279888, -42.53254041760200721 ) ) ;
#941 = ORIENTED_EDGE ( 'NONE', *, *, #4990, .F. ) ;
#942 = AXIS2_PLACEMENT_3D ( 'NONE', #9406, #9328, #14453 ) ;
#943 = AXIS2_PLACEMENT_3D ( 'NONE', #6427, #11487, #8999 ) ;
#944 = CARTESIAN_POINT ( 'NONE',  ( 0.000000000000000000, 262.0000000000000000, 0.000000000000000000 ) ) ;
#945 = CARTESIAN_POINT ( 'NONE',  ( 49.86468353124999453, 37.02187500034138878, -16.20201782572376104 ) ) ;
#946 = CARTESIAN_POINT ( 'NONE',  ( -49.86468353125000164, 19.85937500034139447, 0.000000000000000000 ) ) ;
#947 = PRODUCT_DEFINITION_FORMATION_WITH_SPECIFIED_SOURCE ( 'ANY', '', #7717, .NOT_KNOWN. ) ;
#948 = CARTESIAN_POINT ( 'NONE',  ( 7.580410092413973011, 101.3368000520362813, 5.000000000000000000 ) ) ;
#949 = CARTESIAN_POINT ( 'NONE',  ( 40.34137639590981905, 20.72187500034139873, 29.30972558990010768 ) ) ;
#950 = CARTESIAN_POINT ( 'NONE',  ( -30.90169943749474868, 31.48125000068279533, -42.53254041760200721 ) ) ;
#951 = CARTESIAN_POINT ( 'NONE',  ( 49.86468353125001585, 40.82187500034140726, 16.20201782572375038 ) ) ;
#952 = CARTESIAN_POINT ( 'NONE',  ( -24.93825083352641769, 285.3724546740604637, -7.438250833528329942 ) ) ;
#953 = AXIS2_PLACEMENT_3D ( 'NONE', #5436, #10499, #15557 ) ;
#954 =( GEOMETRIC_REPRESENTATION_CONTEXT ( 3 ) GLOBAL_UNCERTAINTY_ASSIGNED_CONTEXT ( ( #3259 ) ) GLOBAL_UNIT_ASSIGNED_CONTEXT ( ( #12888, #8987, #2830 ) ) REPRESENTATION_CONTEXT ( 'NONE', 'WORKASPACE' ) );
#955 = ORIENTED_EDGE ( 'NONE', *, *, #11085, .F. ) ;
#956 = VECTOR ( 'NONE', #12319, 1000.000000000000000 ) ;
#957 = CARTESIAN_POINT ( 'NONE',  ( 9.631387414534489405E-15, 38.42187500034139447, 52.43083105670540789 ) ) ;
#958 = DIRECTION ( 'NONE',  ( -0.000000000000000000, -1.000000000000000000, -0.000000000000000000 ) ) ;
#959 = ORIENTED_EDGE ( 'NONE', *, *, #281, .F. ) ;
#960 = VERTEX_POINT ( 'NONE', #8246 ) ;
#961 =( BOUNDED_SURFACE ( )  B_SPLINE_SURFACE ( 1, 2, ( 
 ( #234, #12794, #13868, #2484, #5340, #1397, #10392, #3910, #11311, #9138, #15448, #12634, #5013, #4066, #6488, #1236, #15368, #11544, #13949, #14197, #3989, #9061, #12550, #3743, #6330, #476, #15528, #2818, #10640, #9468, #13207, #14520, #7891, #6826, #13121, #4243, #2979, #3143, #5647, #8049, #13045, #1571, #554, #9385, #12966, #13283, #5579, #15617, #11791, #10564, #8136, #10713, #1886, #9309, #11878, #9552, #6977, #10803, #8217, #15692, #5496, #12031, #15773, #15865, #4399, #14435, #633, #6663, #5728, #1728, #312, #391, #4487, #14283, #11956, #11713, #5412, #10470, #4158, #4320, #9230, #2906, #7973, #1647, #14362, #6744, #3058, #1811, #6903, #7307, #1963, #9801, #8463, #8373, #10879, #16021, #13605, #13686, #8294, #9879, #14930, #2210, #12366, #3560, #8613, #2303, #5893, #15941, #968, #11042, #6065, #7391, #13529, #16196, #13446, #13362, #14852, #805, #5810, #9714, #3397, #3222, #16111, #12455, #4824, #2131, #7056, #12120, #11134, #1048, #726, #6143, #7220, #12280, #4744, #2056, #4563, #11215, #16270, #9626, #3480, #882, #5976, #14766, #8535, #14678, #4901, #14599, #3306, #7144, #12203, #10956, #4649, #2633, #9041, #124, #7709, #13771, #6389, #12778, #5239, #1379, #15349, #1212, #10295, #46, #8706, #16352, #6469, #2383, #5150, #3806, #3728, #6221, #11377, #8960, #14096, #3650, #3966, #2710, #14014, #11526, #7790, #12859, #1464, #6308, #11291, #6558, #11452, #11618, #216, #8870, #9959, #8787, #7466, #10207, #12614, #1126, #5074, #15177, #15015, #15259, #12533, #4991, #13931, #10047, #15101, #13849, #2463, #7544, #16440, #2550, #7629, #3888, #10127, #12699, #1298, #1867, #293, #461, #8030, #13104, #371, #10544, #14178, #14418, #5563, #8110, #10624, #10697, #11858, #15428, #2962, #1552, #5319, #1709, #11938, #15678, #539, #10370, #9290, #15602, #6722, #5474, #5633, #13190, #4223, #15507, #4048, #3038, #4304, #9118, #15753, #6806, #1628, #14264, #13026, #9368, #1794, #4381, #11771, #14346, #12016, #9446, #13268, #14500, #6887, #7954, #3129, #8201, #6963, #2795, #7870, #12948, #6645, #11694, #5392, #10451, #4134, #9209, #2885, #9785, #864, #3459, #12263, #6045, #7200, #10779, #14742, #13344, #615, #8443, #7289, #11021, #12345, #5711, #4628, #10937, #2035, #783, #946 ),
 ( #13425, #9611, #8356, #5960, #8520, #11117, #7126, #9690, #7374, #4807, #8595, #16178, #3377, #3287, #9859, #14830, #13668, #13585, #16089, #2192, #4469, #14911, #5875, #14580, #14659, #3541, #12097, #2282, #15845, #9536, #3206, #8278, #13506, #1947, #7040, #704, #5792, #12184, #10859, #4724, #15925, #4547, #16002, #2113, #7612, #6290, #6204, #8688, #13832, #11438, #11512, #6128, #7693, #12763, #31, #5136, #1362, #6453, #108, #3712, #13754, #10191, #8854, #3868, #5215, #11359, #14000, #11275, #11197, #12686, #15085, #3629, #7523, #1190, #1030, #13912, #10275, #2618, #16424, #16250, #4885, #15244, #8942, #9941, #15331, #5060, #10111, #2531, #16333, #14995, #3950, #9024, #7450, #1283, #15162, #8770, #4973, #2446, #6372, #14079, #2694, #12596, #3789, #12437, #2367, #12517, #1107, #10032, #10434, #11922, #5545, #15732, #15663, #14328, #4285, #11599, #6871, #13008, #5302, #275, #522, #2777, #444, #5617, #14399, #10607, #196, #4207, #9349, #3022, #8093, #13168, #15490, #1777, #2945, #6533, #14161, #10680, #10351, #8012, #1611, #1535, #4031, #9184, #6789, #4363, #1445, #9428, #14476, #11833, #7770, #12842, #15413, #9101, #4115, #7850, #12930, #9273, #6624, #11677, #6704, #5379, #14248, #2867, #13086, #7935, #11754, #355, #5455, #10520, #1692, #15582, #9765, #13401, #1849, #8183, #849, #7185, #6945, #14812, #12165, #7110, #4609, #1927, #13249, #4699, #16158, #14564, #14722, #5857, #10921, #14641, #8339, #11999, #12246, #3353, #5941, #8427, #8505, #9672, #595, #767, #15818, #3111, #15983, #3443, #13489, #13570, #5690, #2097, #2013, #4531, #3269, #2174, #11004, #16066, #13325, #10758, #7270, #12326, #4452, #928, #6026, #11098, #4789, #9845, #9517, #3188, #8261, #7020, #12074, #678, #5777, #10843, #15907, #9594, #8576, #237, #11716, #9925, #10093, #1172, #6267, #10010, #3695, #7355, #7811, #15141, #1493, #3769, #4070, #5038, #13651, #12574, #11181, #14897, #11338, #5343, #8828, #10395, #3524, #2426, #8751, #16316, #15066, #15451, #6585, #13814, #8668, #2259, #12882, #13891, #12422, #9142, #16405, #11258, #7432, #6184, #2507, #11642, #14200, #4951, #7503, #5415, #2824, #6666, #7894, #12969, #1092, #1574, #315, #1013, #6110, #16235, #4869, #14979, #3608, #13737, #2350, #12499, #3225 ) ),
 .UNSPECIFIED., .F., .F., .F. ) 
 B_SPLINE_SURFACE_WITH_KNOTS ( ( 2, 2 ),
 ( 3, 2, 2, 2, 2, 2, 2, 2, 2, 2, 2, 2, 2, 2, 2, 2, 2, 2, 2, 2, 2, 2, 2, 2, 2, 2, 2, 2, 2, 2, 2, 2, 2, 2, 2, 2, 2, 2, 2, 2, 2, 2, 2, 2, 2, 2, 2, 2, 2, 2, 2, 2, 2, 2, 2, 2, 2, 2, 2, 2, 2, 2, 2, 2, 2, 2, 2, 2, 2, 2, 2, 2, 2, 2, 2, 2, 2, 2, 2, 2, 2, 2, 2, 2, 2, 2, 2, 2, 2, 2, 2, 2, 2, 2, 2, 2, 2, 2, 2, 2, 2, 2, 2, 2, 2, 2, 2, 2, 2, 2, 2, 2, 2, 2, 2, 2, 2, 2, 2, 2, 2, 2, 2, 2, 2, 2, 2, 2, 2, 2, 2, 2, 2, 2, 2, 2, 2, 2, 2, 2, 2, 2, 2, 2, 2, 2, 2, 2, 2, 2, 3 ),
 ( 0.000000000000000000, 1.000000000000000000 ),
 ( 0.000000000000000000, 0.006666666666666667095, 0.01333333333333333419, 0.02000000000000000042, 0.02666666666666666838, 0.03333333333333333287, 0.04000000000000000083, 0.04666666666666666879, 0.05333333333333333676, 0.05999999999999999778, 0.06666666666666666574, 0.07333333333333333370, 0.08000000000000000167, 0.08666666666666666963, 0.09333333333333333759, 0.1000000000000000056, 0.1066666666666666735, 0.1133333333333333276, 0.1199999999999999956, 0.1266666666666666774, 0.1333333333333333315, 0.1400000000000000133, 0.1466666666666666674, 0.1533333333333333215, 0.1600000000000000033, 0.1666666666666666574, 0.1733333333333333393, 0.1799999999999999933, 0.1866666666666666752, 0.1933333333333333293, 0.2000000000000000111, 0.2066666666666666652, 0.2133333333333333470, 0.2200000000000000011, 0.2266666666666666552, 0.2333333333333333370, 0.2399999999999999911, 0.2466666666666666730, 0.2533333333333333548, 0.2600000000000000089, 0.2666666666666666630, 0.2733333333333333171, 0.2800000000000000266, 0.2866666666666666807, 0.2933333333333333348, 0.2999999999999999889, 0.3066666666666666430, 0.3133333333333333526, 0.3200000000000000067, 0.3266666666666666607, 0.3333333333333333148, 0.3400000000000000244, 0.3466666666666666785, 0.3533333333333333326, 0.3599999999999999867, 0.3666666666666666408, 0.3733333333333333504, 0.3800000000000000044, 0.3866666666666666585, 0.3933333333333333126, 0.4000000000000000222, 0.4066666666666666763, 0.4133333333333333304, 0.4199999999999999845, 0.4266666666666666941, 0.4333333333333333481, 0.4400000000000000022, 0.4466666666666666563, 0.4533333333333333104, 0.4600000000000000200, 0.4666666666666666741, 0.4733333333333333282, 0.4799999999999999822, 0.4866666666666666918, 0.4933333333333333459, 0.5000000000000000000, 0.5066666666666667096, 0.5133333333333333082, 0.5200000000000000178, 0.5266666666666666163, 0.5333333333333333259, 0.5400000000000000355, 0.5466666666666666341, 0.5533333333333333437, 0.5600000000000000533, 0.5666666666666666519, 0.5733333333333333615, 0.5799999999999999600, 0.5866666666666666696, 0.5933333333333333792, 0.5999999999999999778, 0.6066666666666666874, 0.6133333333333332860, 0.6199999999999999956, 0.6266666666666667052, 0.6333333333333333037, 0.6400000000000000133, 0.6466666666666666119, 0.6533333333333333215, 0.6600000000000000311, 0.6666666666666666297, 0.6733333333333333393, 0.6800000000000000488, 0.6866666666666666474, 0.6933333333333333570, 0.6999999999999999556, 0.7066666666666666652, 0.7133333333333333748, 0.7199999999999999734, 0.7266666666666666829, 0.7333333333333332815, 0.7399999999999999911, 0.7466666666666667007, 0.7533333333333332993, 0.7600000000000000089, 0.7666666666666667185, 0.7733333333333333171, 0.7800000000000000266, 0.7866666666666666252, 0.7933333333333333348, 0.8000000000000000444, 0.8066666666666666430, 0.8133333333333333526, 0.8199999999999999512, 0.8266666666666666607, 0.8333333333333333703, 0.8399999999999999689, 0.8466666666666666785, 0.8533333333333333881, 0.8599999999999999867, 0.8666666666666666963, 0.8733333333333332948, 0.8800000000000000044, 0.8866666666666667140, 0.8933333333333333126, 0.9000000000000000222, 0.9066666666666666208, 0.9133333333333333304, 0.9200000000000000400, 0.9266666666666666385, 0.9333333333333333481, 0.9399999999999999467, 0.9466666666666666563, 0.9533333333333333659, 0.9599999999999999645, 0.9666666666666666741, 0.9733333333333333837, 0.9799999999999999822, 0.9866666666666666918, 0.9933333333333332904, 1.000000000000000000 ),
 .UNSPECIFIED. ) 
 GEOMETRIC_REPRESENTATION_ITEM ( )  RATIONAL_B_SPLINE_SURFACE ( (
 ( 1.000000000000000000, 0.9510565162951535312, 1.000000000000000000, 0.9510565162951535312, 1.000000000000000000, 0.9510565162951535312, 1.000000000000000000, 0.9510565162951535312, 1.000000000000000000, 0.9510565162951535312, 1.000000000000000000, 0.9510565162951535312, 1.000000000000000000, 0.9510565162951535312, 1.000000000000000000, 0.9510565162951535312, 1.000000000000000000, 0.9510565162951535312, 1.000000000000000000, 0.9510565162951535312, 1.000000000000000000, 0.9510565162951535312, 1.000000000000000000, 0.9510565162951535312, 1.000000000000000000, 0.9510565162951535312, 1.000000000000000000, 0.9510565162951535312, 1.000000000000000000, 0.9510565162951535312, 1.000000000000000000, 0.9510565162951535312, 1.000000000000000000, 0.9510565162951535312, 1.000000000000000000, 0.9510565162951535312, 1.000000000000000000, 0.9510565162951535312, 1.000000000000000000, 0.9510565162951535312, 1.000000000000000000, 0.9510565162951535312, 1.000000000000000000, 0.9510565162951535312, 1.000000000000000000, 0.9510565162951535312, 1.000000000000000000, 0.9510565162951535312, 1.000000000000000000, 0.9510565162951535312, 1.000000000000000000, 0.9510565162951535312, 1.000000000000000000, 0.9510565162951535312, 1.000000000000000000, 0.9510565162951535312, 1.000000000000000000, 0.9510565162951535312, 1.000000000000000000, 0.9510565162951535312, 1.000000000000000000, 0.9510565162951535312, 1.000000000000000000, 0.9510565162951535312, 1.000000000000000000, 0.9510565162951535312, 1.000000000000000000, 0.9510565162951535312, 1.000000000000000000, 0.9510565162951535312, 1.000000000000000000, 0.9510565162951535312, 1.000000000000000000, 0.9510565162951535312, 1.000000000000000000, 0.9510565162951535312, 1.000000000000000000, 0.9510565162951535312, 1.000000000000000000, 0.9510565162951535312, 1.000000000000000000, 0.9510565162951535312, 1.000000000000000000, 0.9510565162951535312, 1.000000000000000000, 0.9510565162951535312, 1.000000000000000000, 0.9510565162951535312, 1.000000000000000000, 0.9510565162951535312, 1.000000000000000000, 0.9510565162951535312, 1.000000000000000000, 0.9510565162951535312, 1.000000000000000000, 0.9510565162951535312, 1.000000000000000000, 0.9510565162951535312, 1.000000000000000000, 0.9510565162951535312, 1.000000000000000000, 0.9510565162951535312, 1.000000000000000000, 0.9510565162951535312, 1.000000000000000000, 0.9510565162951535312, 1.000000000000000000, 0.9510565162951535312, 1.000000000000000000, 0.9510565162951535312, 1.000000000000000000, 0.9510565162951535312, 1.000000000000000000, 0.9510565162951535312, 1.000000000000000000, 0.9510565162951535312, 1.000000000000000000, 0.9510565162951535312, 1.000000000000000000, 0.9510565162951535312, 1.000000000000000000, 0.9510565162951535312, 1.000000000000000000, 0.9510565162951535312, 1.000000000000000000, 0.9510565162951535312, 1.000000000000000000, 0.9510565162951535312, 1.000000000000000000, 0.9510565162951535312, 1.000000000000000000, 0.9510565162951535312, 1.000000000000000000, 0.9510565162951535312, 1.000000000000000000, 0.9510565162951535312, 1.000000000000000000, 0.9510565162951535312, 1.000000000000000000, 0.9510565162951535312, 1.000000000000000000, 0.9510565162951535312, 1.000000000000000000, 0.9510565162951535312, 1.000000000000000000, 0.9510565162951535312, 1.000000000000000000, 0.9510565162951535312, 1.000000000000000000, 0.9510565162951535312, 1.000000000000000000, 0.9510565162951535312, 1.000000000000000000, 0.9510565162951535312, 1.000000000000000000, 0.9510565162951535312, 1.000000000000000000, 0.9510565162951535312, 1.000000000000000000, 0.9510565162951535312, 1.000000000000000000, 0.9510565162951535312, 1.000000000000000000, 0.9510565162951535312, 1.000000000000000000, 0.9510565162951535312, 1.000000000000000000, 0.9510565162951535312, 1.000000000000000000, 0.9510565162951535312, 1.000000000000000000, 0.9510565162951535312, 1.000000000000000000, 0.9510565162951535312, 1.000000000000000000, 0.9510565162951535312, 1.000000000000000000, 0.9510565162951535312, 1.000000000000000000, 0.9510565162951535312, 1.000000000000000000, 0.9510565162951535312, 1.000000000000000000, 0.9510565162951535312, 1.000000000000000000, 0.9510565162951535312, 1.000000000000000000, 0.9510565162951535312, 1.000000000000000000, 0.9510565162951535312, 1.000000000000000000, 0.9510565162951535312, 1.000000000000000000, 0.9510565162951535312, 1.000000000000000000, 0.9510565162951535312, 1.000000000000000000, 0.9510565162951535312, 1.000000000000000000, 0.9510565162951535312, 1.000000000000000000, 0.9510565162951535312, 1.000000000000000000, 0.9510565162951535312, 1.000000000000000000, 0.9510565162951535312, 1.000000000000000000, 0.9510565162951535312, 1.000000000000000000, 0.9510565162951535312, 1.000000000000000000, 0.9510565162951535312, 1.000000000000000000, 0.9510565162951535312, 1.000000000000000000, 0.9510565162951535312, 1.000000000000000000, 0.9510565162951535312, 1.000000000000000000, 0.9510565162951535312, 1.000000000000000000, 0.9510565162951535312, 1.000000000000000000, 0.9510565162951535312, 1.000000000000000000, 0.9510565162951535312, 1.000000000000000000, 0.9510565162951535312, 1.000000000000000000, 0.9510565162951535312, 1.000000000000000000, 0.9510565162951535312, 1.000000000000000000, 0.9510565162951535312, 1.000000000000000000, 0.9510565162951535312, 1.000000000000000000, 0.9510565162951535312, 1.000000000000000000, 0.9510565162951535312, 1.000000000000000000, 0.9510565162951535312, 1.000000000000000000, 0.9510565162951535312, 1.000000000000000000, 0.9510565162951535312, 1.000000000000000000, 0.9510565162951535312, 1.000000000000000000, 0.9510565162951535312, 1.000000000000000000, 0.9510565162951535312, 1.000000000000000000, 0.9510565162951535312, 1.000000000000000000, 0.9510565162951535312, 1.000000000000000000, 0.9510565162951535312, 1.000000000000000000, 0.9510565162951535312, 1.000000000000000000, 0.9510565162951535312, 1.000000000000000000, 0.9510565162951535312, 1.000000000000000000, 0.9510565162951535312, 1.000000000000000000, 0.9510565162951535312, 1.000000000000000000, 0.9510565162951535312, 1.000000000000000000, 0.9510565162951535312, 1.000000000000000000, 0.9510565162951535312, 1.000000000000000000, 0.9510565162951535312, 1.000000000000000000, 0.9510565162951535312, 1.000000000000000000, 0.9510565162951535312, 1.000000000000000000, 0.9510565162951535312, 1.000000000000000000, 0.9510565162951535312, 1.000000000000000000, 0.9510565162951535312, 1.000000000000000000, 0.9510565162951535312, 1.000000000000000000, 0.9510565162951535312, 1.000000000000000000, 0.9510565162951535312, 1.000000000000000000, 0.9510565162951535312, 1.000000000000000000, 0.9510565162951535312, 1.000000000000000000, 0.9510565162951535312, 1.000000000000000000, 0.9510565162951535312, 1.000000000000000000),
 ( 1.000000000000000000, 0.9510565162951535312, 1.000000000000000000, 0.9510565162951535312, 1.000000000000000000, 0.9510565162951535312, 1.000000000000000000, 0.9510565162951535312, 1.000000000000000000, 0.9510565162951535312, 1.000000000000000000, 0.9510565162951535312, 1.000000000000000000, 0.9510565162951535312, 1.000000000000000000, 0.9510565162951535312, 1.000000000000000000, 0.9510565162951535312, 1.000000000000000000, 0.9510565162951535312, 1.000000000000000000, 0.9510565162951535312, 1.000000000000000000, 0.9510565162951535312, 1.000000000000000000, 0.9510565162951535312, 1.000000000000000000, 0.9510565162951535312, 1.000000000000000000, 0.9510565162951535312, 1.000000000000000000, 0.9510565162951535312, 1.000000000000000000, 0.9510565162951535312, 1.000000000000000000, 0.9510565162951535312, 1.000000000000000000, 0.9510565162951535312, 1.000000000000000000, 0.9510565162951535312, 1.000000000000000000, 0.9510565162951535312, 1.000000000000000000, 0.9510565162951535312, 1.000000000000000000, 0.9510565162951535312, 1.000000000000000000, 0.9510565162951535312, 1.000000000000000000, 0.9510565162951535312, 1.000000000000000000, 0.9510565162951535312, 1.000000000000000000, 0.9510565162951535312, 1.000000000000000000, 0.9510565162951535312, 1.000000000000000000, 0.9510565162951535312, 1.000000000000000000, 0.9510565162951535312, 1.000000000000000000, 0.9510565162951535312, 1.000000000000000000, 0.9510565162951535312, 1.000000000000000000, 0.9510565162951535312, 1.000000000000000000, 0.9510565162951535312, 1.000000000000000000, 0.9510565162951535312, 1.000000000000000000, 0.9510565162951535312, 1.000000000000000000, 0.9510565162951535312, 1.000000000000000000, 0.9510565162951535312, 1.000000000000000000, 0.9510565162951535312, 1.000000000000000000, 0.9510565162951535312, 1.000000000000000000, 0.9510565162951535312, 1.000000000000000000, 0.9510565162951535312, 1.000000000000000000, 0.9510565162951535312, 1.000000000000000000, 0.9510565162951535312, 1.000000000000000000, 0.9510565162951535312, 1.000000000000000000, 0.9510565162951535312, 1.000000000000000000, 0.9510565162951535312, 1.000000000000000000, 0.9510565162951535312, 1.000000000000000000, 0.9510565162951535312, 1.000000000000000000, 0.9510565162951535312, 1.000000000000000000, 0.9510565162951535312, 1.000000000000000000, 0.9510565162951535312, 1.000000000000000000, 0.9510565162951535312, 1.000000000000000000, 0.9510565162951535312, 1.000000000000000000, 0.9510565162951535312, 1.000000000000000000, 0.9510565162951535312, 1.000000000000000000, 0.9510565162951535312, 1.000000000000000000, 0.9510565162951535312, 1.000000000000000000, 0.9510565162951535312, 1.000000000000000000, 0.9510565162951535312, 1.000000000000000000, 0.9510565162951535312, 1.000000000000000000, 0.9510565162951535312, 1.000000000000000000, 0.9510565162951535312, 1.000000000000000000, 0.9510565162951535312, 1.000000000000000000, 0.9510565162951535312, 1.000000000000000000, 0.9510565162951535312, 1.000000000000000000, 0.9510565162951535312, 1.000000000000000000, 0.9510565162951535312, 1.000000000000000000, 0.9510565162951535312, 1.000000000000000000, 0.9510565162951535312, 1.000000000000000000, 0.9510565162951535312, 1.000000000000000000, 0.9510565162951535312, 1.000000000000000000, 0.9510565162951535312, 1.000000000000000000, 0.9510565162951535312, 1.000000000000000000, 0.9510565162951535312, 1.000000000000000000, 0.9510565162951535312, 1.000000000000000000, 0.9510565162951535312, 1.000000000000000000, 0.9510565162951535312, 1.000000000000000000, 0.9510565162951535312, 1.000000000000000000, 0.9510565162951535312, 1.000000000000000000, 0.9510565162951535312, 1.000000000000000000, 0.9510565162951535312, 1.000000000000000000, 0.9510565162951535312, 1.000000000000000000, 0.9510565162951535312, 1.000000000000000000, 0.9510565162951535312, 1.000000000000000000, 0.9510565162951535312, 1.000000000000000000, 0.9510565162951535312, 1.000000000000000000, 0.9510565162951535312, 1.000000000000000000, 0.9510565162951535312, 1.000000000000000000, 0.9510565162951535312, 1.000000000000000000, 0.9510565162951535312, 1.000000000000000000, 0.9510565162951535312, 1.000000000000000000, 0.9510565162951535312, 1.000000000000000000, 0.9510565162951535312, 1.000000000000000000, 0.9510565162951535312, 1.000000000000000000, 0.9510565162951535312, 1.000000000000000000, 0.9510565162951535312, 1.000000000000000000, 0.9510565162951535312, 1.000000000000000000, 0.9510565162951535312, 1.000000000000000000, 0.9510565162951535312, 1.000000000000000000, 0.9510565162951535312, 1.000000000000000000, 0.9510565162951535312, 1.000000000000000000, 0.9510565162951535312, 1.000000000000000000, 0.9510565162951535312, 1.000000000000000000, 0.9510565162951535312, 1.000000000000000000, 0.9510565162951535312, 1.000000000000000000, 0.9510565162951535312, 1.000000000000000000, 0.9510565162951535312, 1.000000000000000000, 0.9510565162951535312, 1.000000000000000000, 0.9510565162951535312, 1.000000000000000000, 0.9510565162951535312, 1.000000000000000000, 0.9510565162951535312, 1.000000000000000000, 0.9510565162951535312, 1.000000000000000000, 0.9510565162951535312, 1.000000000000000000, 0.9510565162951535312, 1.000000000000000000, 0.9510565162951535312, 1.000000000000000000, 0.9510565162951535312, 1.000000000000000000, 0.9510565162951535312, 1.000000000000000000, 0.9510565162951535312, 1.000000000000000000, 0.9510565162951535312, 1.000000000000000000, 0.9510565162951535312, 1.000000000000000000, 0.9510565162951535312, 1.000000000000000000, 0.9510565162951535312, 1.000000000000000000, 0.9510565162951535312, 1.000000000000000000, 0.9510565162951535312, 1.000000000000000000, 0.9510565162951535312, 1.000000000000000000, 0.9510565162951535312, 1.000000000000000000, 0.9510565162951535312, 1.000000000000000000, 0.9510565162951535312, 1.000000000000000000, 0.9510565162951535312, 1.000000000000000000, 0.9510565162951535312, 1.000000000000000000, 0.9510565162951535312, 1.000000000000000000, 0.9510565162951535312, 1.000000000000000000, 0.9510565162951535312, 1.000000000000000000, 0.9510565162951535312, 1.000000000000000000, 0.9510565162951535312, 1.000000000000000000, 0.9510565162951535312, 1.000000000000000000, 0.9510565162951535312, 1.000000000000000000, 0.9510565162951535312, 1.000000000000000000, 0.9510565162951535312, 1.000000000000000000, 0.9510565162951535312, 1.000000000000000000, 0.9510565162951535312, 1.000000000000000000, 0.9510565162951535312, 1.000000000000000000, 0.9510565162951535312, 1.000000000000000000, 0.9510565162951535312, 1.000000000000000000, 0.9510565162951535312, 1.000000000000000000, 0.9510565162951535312, 1.000000000000000000, 0.9510565162951535312, 1.000000000000000000, 0.9510565162951535312, 1.000000000000000000, 0.9510565162951535312, 1.000000000000000000) ) ) 
 REPRESENTATION_ITEM ( '' )  SURFACE ( )  );
#962 = ORIENTED_EDGE ( 'NONE', *, *, #15661, .F. ) ;
#963 = EDGE_CURVE ( 'NONE', #14610, #15483, #2393, .T. ) ;
#964 = CARTESIAN_POINT ( 'NONE',  ( -49.99999999999999289, 39.88125000068280457, 16.24598481164533226 ) ) ;
#965 = CARTESIAN_POINT ( 'NONE',  ( 9.297345850538470396E-15, 92.00000000000001421, -1.969248798088869855E-14 ) ) ;
#966 = CARTESIAN_POINT ( 'NONE',  ( -49.99999999999999289, 49.89999999999999147, -16.24598481164531449 ) ) ;
#967 = CARTESIAN_POINT ( 'NONE',  ( 7.919222016226875382, 37.22999571913595673, -49.99999999999997158 ) ) ;
#968 = CARTESIAN_POINT ( 'NONE',  ( 40.34137639590981195, 39.05937500034140442, -29.30972558990011834 ) ) ;
#969 = VECTOR ( 'NONE', #3869, 1000.000000000000000 ) ;
#970 = CARTESIAN_POINT ( 'NONE',  ( 49.86468353125000164, 44.85937500034140157, -6.106662507704105588E-15 ) ) ;
#971 = CARTESIAN_POINT ( 'NONE',  ( 0.000000000000000000, 25.00000000000000000, 0.000000000000000000 ) ) ;
#972 = AXIS2_PLACEMENT_3D ( 'NONE', #1664, #10655, #11808 ) ;
#973 = CARTESIAN_POINT ( 'NONE',  ( -49.86468353124999453, 49.82187500034139305, -16.20201782572375393 ) ) ;
#974 = DIRECTION ( 'NONE',  ( 0.000000000000000000, 0.000000000000000000, -1.000000000000000000 ) ) ;
#975 = CARTESIAN_POINT ( 'NONE',  ( 1.293669679204937499E-13, 41.50000000000000000, -50.00000000000000000 ) ) ;
#976 =( LENGTH_UNIT ( ) NAMED_UNIT ( * ) SI_UNIT ( .MILLI., .METRE. ) );
#977 = ORIENTED_EDGE ( 'NONE', *, *, #9370, .T. ) ;
#978 = CARTESIAN_POINT ( 'NONE',  ( -49.86468353124999453, 21.75937500034140015, -16.20201782572375393 ) ) ;
#979 = AXIS2_PLACEMENT_3D ( 'NONE', #3337, #9656, #12404 ) ;
#980 = EDGE_LOOP ( 'NONE', ( #7460, #8207, #4357, #5512 ) ) ;
#981 = ORIENTED_EDGE ( 'NONE', *, *, #4267, .T. ) ;
#982 = VERTEX_POINT ( 'NONE', #15894 ) ;
#983 = CARTESIAN_POINT ( 'NONE',  ( -49.99999999999999289, 45.88125000068279746, 16.24598481164533226 ) ) ;
#984 = CARTESIAN_POINT ( 'NONE',  ( -1.240322475938754499E-13, 40.50000000000000000, 50.00000000000000000 ) ) ;
#985 = ORIENTED_EDGE ( 'NONE', *, *, #3765, .T. ) ;
#986 = CARTESIAN_POINT ( 'NONE',  ( 1.293669679204937499E-13, 39.28125000068280315, -50.00000000000000000 ) ) ;
#987 =( NAMED_UNIT ( * ) PLANE_ANGLE_UNIT ( ) SI_UNIT ( $, .RADIAN. ) );
#988 = CARTESIAN_POINT ( 'NONE',  ( -14.89909204896622263, 13.30277682295380615, 96.51165749809530325 ) ) ;
#989 = CARTESIAN_POINT ( 'NONE',  ( -16.16503364901097939, 28.27806893495044349, 101.3333374614808662 ) ) ;
#990 = CARTESIAN_POINT ( 'NONE',  ( 0.000000000000000000, 20.00000000000000355, 0.000000000000000000 ) ) ;
#991 = DIRECTION ( 'NONE',  ( -0.9961946980917455452, -0.08715574274765824914, 0.000000000000000000 ) ) ;
#992 = FACE_OUTER_BOUND ( 'NONE', #13500, .T. ) ;
#993 = CARTESIAN_POINT ( 'NONE',  ( 40.45084971874737789, 36.58125000068280031, 29.38926261462365375 ) ) ;
#994 = CARTESIAN_POINT ( 'NONE',  ( -49.99999999999999289, 41.90000000000000568, -16.24598481164531449 ) ) ;
#995 = CARTESIAN_POINT ( 'NONE',  ( 15.45084971874737789, 46.38125000068279746, 47.55282581475767500 ) ) ;
#996 = CARTESIAN_POINT ( 'NONE',  ( 0.000000000000000000, 22.50000000000000000, 101.0000000000000000 ) ) ;
#997 = CARTESIAN_POINT ( 'NONE',  ( -15.45084971874737256, 31.60000000000000142, -47.55282581475767500 ) ) ;
#998 = CARTESIAN_POINT ( 'NONE',  ( -30.90169943749473447, 26.29999999999999716, 42.53254041760200721 ) ) ;
#999 = DIRECTION ( 'NONE',  ( 0.9961946980917455452, 0.08715574274765823526, -0.000000000000000000 ) ) ;
#1000 = CARTESIAN_POINT ( 'NONE',  ( -3.210462471511496205E-15, 43.35937500034138736, -52.43083105670540789 ) ) ;
#1001 = VERTEX_POINT ( 'NONE', #7172 ) ;
#1002 = EDGE_CURVE ( 'NONE', #11153, #15748, #13312, .T. ) ;
#1003 = CARTESIAN_POINT ( 'NONE',  ( -25.00000000000000711, 284.0710678118655323, -2.499999999999999556 ) ) ;
#1004 = EDGE_LOOP ( 'NONE', ( #10265, #9223, #9244, #3240 ) ) ;
#1005 = LINE ( 'NONE', #8661, #11852 ) ;
#1006 = CARTESIAN_POINT ( 'NONE',  ( 49.86468353125000164, 32.85937500034139447, -6.106662507704105588E-15 ) ) ;
#1007 = CARTESIAN_POINT ( 'NONE',  ( 14.61046079763427130, 13.48729625631194118, 101.3333374614808662 ) ) ;
#1009 = EDGE_CURVE ( 'NONE', #14610, #7079, #9830, .T. ) ;
#1008 = DIRECTION ( 'NONE',  ( 0.000000000000000000, -5.551115123125782702E-17, 1.000000000000000000 ) ) ;
#1010 = PRODUCT_RELATED_PRODUCT_CATEGORY ( 'part', '', ( #8125 ) ) ;
#1011 = CARTESIAN_POINT ( 'NONE',  ( 50.00000000000000000, 35.00000000000000000, -6.123233995736766085E-15 ) ) ;
#1012 = CARTESIAN_POINT ( 'NONE',  ( 40.45084971874737079, 44.98125000068279888, -29.38926261462366440 ) ) ;
#1013 = CARTESIAN_POINT ( 'NONE',  ( 49.86468353125001585, 20.82187500034140015, 16.20201782572375038 ) ) ;
#1014 = CARTESIAN_POINT ( 'NONE',  ( 9.631387414534489405E-15, 32.35937500034139447, 52.43083105670540789 ) ) ;
#1015 = CARTESIAN_POINT ( 'NONE',  ( -7.919222016226816763, 35.55125428154684641, -49.99999999999999289 ) ) ;
#1016 = CARTESIAN_POINT ( 'NONE',  ( -49.86468353125000164, 35.92187500034140157, 0.000000000000000000 ) ) ;
#1017 = CARTESIAN_POINT ( 'NONE',  ( 0.000000000000000000, 20.00000000000000355, 0.000000000000000000 ) ) ;
#1018 = VECTOR ( 'NONE', #4511, 1000.000000000000000 ) ;
#1019 = ADVANCED_FACE ( 'NONE', ( #14880 ), #4591, .T. ) ;
#1020 = CARTESIAN_POINT ( 'NONE',  ( -40.34137639590981195, 38.05937500034139731, 29.30972558990012189 ) ) ;
#1021 = CARTESIAN_POINT ( 'NONE',  ( 40.34137639590981195, 37.12187500034139731, -29.30972558990011834 ) ) ;
#1022 = CARTESIAN_POINT ( 'NONE',  ( 50.00000000000000000, 45.00000000000000711, -6.123233995736766085E-15 ) ) ;
#1023 = ORIENTED_EDGE ( 'NONE', *, *, #9637, .F. ) ;
#1024 = ADVANCED_FACE ( 'NONE', ( #5926 ), #3253, .T. ) ;
#1025 = CARTESIAN_POINT ( 'NONE',  ( -49.86468353125000164, 41.85937500034139447, 0.000000000000000000 ) ) ;
#1026 = EDGE_LOOP ( 'NONE', ( #3436, #11766, #12269, #6841, #5637 ) ) ;
#1027 = CARTESIAN_POINT ( 'NONE',  ( -40.45084971874737789, 21.58125000068279675, -29.38926261462365730 ) ) ;
#1028 = ORIENTED_EDGE ( 'NONE', *, *, #8675, .T. ) ;
#1029 = CARTESIAN_POINT ( 'NONE',  ( -1.240322475938754499E-13, 40.28125000068280315, 50.00000000000000000 ) ) ;
#1030 = CARTESIAN_POINT ( 'NONE',  ( 15.40903463028482356, 42.52187500034139589, 47.42413220539093999 ) ) ;
#1031 = FACE_OUTER_BOUND ( 'NONE', #11108, .T. ) ;
#1032 = CARTESIAN_POINT ( 'NONE',  ( 49.86468353125000164, 22.92187500034139802, -6.106662507704105588E-15 ) ) ;
#1033 = ADVANCED_FACE ( 'NONE', ( #14549 ), #10907, .F. ) ;
#1034 = CARTESIAN_POINT ( 'NONE',  ( 15.45084971874736723, 37.18125000068280173, -47.55282581475768211 ) ) ;
#1035 = CARTESIAN_POINT ( 'NONE',  ( -49.86468353125000164, 35.92187500034140157, 0.000000000000000000 ) ) ;
#1036 = CARTESIAN_POINT ( 'NONE',  ( -26.95005104082770231, 283.0244618719127629, -6.400102081653810338 ) ) ;
#1037 = ADVANCED_FACE ( 'NONE', ( #12061 ), #4680, .T. ) ;
#1038 = CARTESIAN_POINT ( 'NONE',  ( -15.40903463028481646, 37.52187500034139589, -47.42413220539093999 ) ) ;
#1039 = FACE_OUTER_BOUND ( 'NONE', #9562, .T. ) ;
#1040 = EDGE_LOOP ( 'NONE', ( #13375, #11613, #1901, #5104 ) ) ;
#1041 = ORIENTED_EDGE ( 'NONE', *, *, #14423, .T. ) ;
#1042 = VERTEX_POINT ( 'NONE', #14706 ) ;
#1043 = DIRECTION ( 'NONE',  ( 0.000000000000000000, 0.000000000000000000, 1.000000000000000000 ) ) ;
#1044 = LINE ( 'NONE', #12452, #15798 ) ;
#1045 = CARTESIAN_POINT ( 'NONE',  ( 30.90169943749473802, 27.29999999999999716, -42.53254041760200721 ) ) ;
#1046 = CARTESIAN_POINT ( 'NONE',  ( -40.45084971874737789, 23.58125000068280031, -29.38926261462365730 ) ) ;
#1047 = CIRCLE ( 'NONE', #1583, 2.267949192431125027 ) ;
#1048 = CARTESIAN_POINT ( 'NONE',  ( 49.86468353124999453, 36.95937500034139589, -16.20201782572376459 ) ) ;
#1049 = EDGE_CURVE ( 'NONE', #3882, #11932, #14795, .T. ) ;
#1050 = CARTESIAN_POINT ( 'NONE',  ( -3.210462471511496205E-15, 45.35937500034139447, -52.43083105670540789 ) ) ;
#1051 = SURFACE_STYLE_USAGE ( .BOTH. , #4992 ) ;
#1052 = CARTESIAN_POINT ( 'NONE',  ( -15.53071739328007794, 28.07196708982276334, 102.0000000000000142 ) ) ;
#1053 = DIRECTION ( 'NONE',  ( 0.000000000000000000, 0.000000000000000000, 1.000000000000000000 ) ) ;
#1054 = FACE_OUTER_BOUND ( 'NONE', #13700, .T. ) ;
#1055 = CARTESIAN_POINT ( 'NONE',  ( 40.45084971874737789, 40.80000000000000426, 29.38926261462365375 ) ) ;
#1056 = CARTESIAN_POINT ( 'NONE',  ( 7.500000000000000000, 40.00000000000000711, 39.29058411375427795 ) ) ;
#1057 = EDGE_LOOP ( 'NONE', ( #1893, #7443, #15977, #14426 ) ) ;
#1058 =( BOUNDED_CURVE ( )  B_SPLINE_CURVE ( 3, ( #2059, #3401, #4566, #11138 ),
 .UNSPECIFIED., .F., .F. ) 
 B_SPLINE_CURVE_WITH_KNOTS ( ( 4, 4 ),
 ( 1.570796326794896780, 3.141592653589793116 ),
 .UNSPECIFIED. ) 
 CURVE ( )  GEOMETRIC_REPRESENTATION_ITEM ( )  RATIONAL_B_SPLINE_CURVE ( ( 1.000000000000000000, 0.8047378541243650485, 0.8047378541243650485, 1.000000000000000000 ) ) 
 REPRESENTATION_ITEM ( '' )  );
#1059 = CARTESIAN_POINT ( 'NONE',  ( 40.34137639590981195, 27.05937500034139731, -29.30972558990011834 ) ) ;
#1060 = EDGE_LOOP ( 'NONE', ( #3862, #4804, #10733, #13726 ) ) ;
#1061 = ORIENTED_EDGE ( 'NONE', *, *, #9175, .F. ) ;
#1062 = VERTEX_POINT ( 'NONE', #8489 ) ;
#1063 = CARTESIAN_POINT ( 'NONE',  ( -15.45084971874737256, 39.38125000068279746, -47.55282581475767500 ) ) ;
#1064 = CARTESIAN_POINT ( 'NONE',  ( 15.45084971874736723, 47.40000000000000568, -47.55282581475768211 ) ) ;
#1065 = CARTESIAN_POINT ( 'NONE',  ( 0.000000000000000000, 0.000000000000000000, 5.000000000000000000 ) ) ;
#1066 = ORIENTED_EDGE ( 'NONE', *, *, #4920, .T. ) ;
#1067 = CARTESIAN_POINT ( 'NONE',  ( 8.660254037844387298, 28.00000000000000355, 5.000000000000000000 ) ) ;
#1068 = CARTESIAN_POINT ( 'NONE',  ( -40.45084971874737079, 38.20000000000000284, 29.38926261462367151 ) ) ;
#1069 = CARTESIAN_POINT ( 'NONE',  ( -14.27211209225524158, 12.35708747557853826, 96.77492152178915319 ) ) ;
#1070 = LINE ( 'NONE', #6161, #12897 ) ;
#1071 = CARTESIAN_POINT ( 'NONE',  ( -4.999999999999995559, 126.6482322781408953, 36.06244584051386681 ) ) ;
#1072 = DIRECTION ( 'NONE',  ( -0.000000000000000000, -1.000000000000000000, -0.000000000000000000 ) ) ;
#1073 = DIRECTION ( 'NONE',  ( 0.000000000000000000, 0.000000000000000000, 1.000000000000000000 ) ) ;
#1074 = PRESENTATION_STYLE_ASSIGNMENT (( #12482 ) ) ;
#1075 = DIRECTION ( 'NONE',  ( -0.000000000000000000, -1.000000000000000000, -0.000000000000000000 ) ) ;
#1076 = CARTESIAN_POINT ( 'NONE',  ( 30.90169943749474157, 47.08125000068280031, -42.53254041760200721 ) ) ;
#1077 = DIRECTION ( 'NONE',  ( -0.000000000000000000, -1.000000000000000000, -0.000000000000000000 ) ) ;
#1078 = CARTESIAN_POINT ( 'NONE',  ( 40.45084971874737789, 28.80000000000000426, 29.38926261462365375 ) ) ;
#1079 = ADVANCED_FACE ( 'NONE', ( #8408 ), #911, .F. ) ;
#1080 = CARTESIAN_POINT ( 'NONE',  ( -15.45084971874737256, 25.60000000000000142, -47.55282581475767500 ) ) ;
#1081 = LINE ( 'NONE', #7492, #677 ) ;
#1082 = CARTESIAN_POINT ( 'NONE',  ( -30.81806926056962226, 46.15937500034139873, 42.41743335407647919 ) ) ;
#1083 = VERTEX_POINT ( 'NONE', #4517 ) ;
#1084 = CARTESIAN_POINT ( 'NONE',  ( -5.026048470455315886, 27.47395152954465658, 39.76282541253125657 ) ) ;
#1085 = ORIENTED_EDGE ( 'NONE', *, *, #15147, .F. ) ;
#1086 = DIRECTION ( 'NONE',  ( -0.8660254037844433705, 0.4999999999999918954, 0.000000000000000000 ) ) ;
#1087 = CARTESIAN_POINT ( 'NONE',  ( -15.40903463028480580, 34.25937500034139305, 47.42413220539094709 ) ) ;
#1088 = CARTESIAN_POINT ( 'NONE',  ( -7.919222016226934890, 20.22999571913595318, 49.99999999999996447 ) ) ;
#1089 = DIRECTION ( 'NONE',  ( -0.000000000000000000, 1.000000000000000000, -0.000000000000000000 ) ) ;
#1090 = CARTESIAN_POINT ( 'NONE',  ( 47.74744883082096436, 24.99999999999999289, -14.37691108325706679 ) ) ;
#1091 = CARTESIAN_POINT ( 'NONE',  ( 49.99999999999999289, 46.88125000068279036, -16.24598481164532160 ) ) ;
#1092 = CARTESIAN_POINT ( 'NONE',  ( 40.34137639590981195, 21.12187500034139376, -29.30972558990011834 ) ) ;
#1093 = CARTESIAN_POINT ( 'NONE',  ( -40.34137639590981195, 30.05937500034139731, 29.30972558990012189 ) ) ;
#1094 = PLANE ( 'NONE',  #12119 ) ;
#1095 = CARTESIAN_POINT ( 'NONE',  ( 30.81806926056962936, 33.22187500034139163, -42.41743335407646498 ) ) ;
#1096 = CARTESIAN_POINT ( 'NONE',  ( -15.45084971874736368, 40.40000000000000568, 47.55282581475768211 ) ) ;
#1097 = CARTESIAN_POINT ( 'NONE',  ( 49.86468353125001585, 40.75937500034138594, 16.20201782572375038 ) ) ;
#1098 = CARTESIAN_POINT ( 'NONE',  ( -30.81806926056962226, 36.22187500034139873, 42.41743335407647919 ) ) ;
#1099 = CARTESIAN_POINT ( 'NONE',  ( 49.99999999999999289, 43.10000000000000142, -16.24598481164532160 ) ) ;
#1100 = EDGE_CURVE ( 'NONE', #1499, #2544, #12417, .T. ) ;
#1101 = VERTEX_POINT ( 'NONE', #7092 ) ;
#1102 = CARTESIAN_POINT ( 'NONE',  ( -15.40903463028481646, 41.45937500034140299, -47.42413220539093999 ) ) ;
#1103 = ORIENTED_EDGE ( 'NONE', *, *, #11803, .F. ) ;
#1104 = CARTESIAN_POINT ( 'NONE',  ( 40.45084971874737789, 22.58125000068279675, 29.38926261462365375 ) ) ;
#1105 = LINE ( 'NONE', #13997, #5701 ) ;
#1106 = FACE_OUTER_BOUND ( 'NONE', #13659, .T. ) ;
#1107 = CARTESIAN_POINT ( 'NONE',  ( 15.40903463028481113, 39.32187500034140015, -47.42413220539094709 ) ) ;
#1108 = CARTESIAN_POINT ( 'NONE',  ( -2.547328955960238000E-13, 30.49999999999999645, 49.99999999999999289 ) ) ;
#1109 = ADVANCED_FACE ( 'NONE', ( #13477 ), #12152, .T. ) ;
#1110 = CARTESIAN_POINT ( 'NONE',  ( 30.81806926056964002, 24.62187500034139731, 42.41743335407647209 ) ) ;
#1111 = CARTESIAN_POINT ( 'NONE',  ( 49.99999999999999289, 30.88125000068279391, -16.24598481164532160 ) ) ;
#1112 = EDGE_CURVE ( 'NONE', #860, #7211, #5048, .T. ) ;
#1113 = CARTESIAN_POINT ( 'NONE',  ( -49.86468353125000164, 31.92187500034139447, 0.000000000000000000 ) ) ;
#1114 = CARTESIAN_POINT ( 'NONE',  ( -24.96465690379244862, 286.9981936728224241, -7.464656903793316367 ) ) ;
#1115 = ADVANCED_FACE ( 'NONE', ( #1155 ), #12485, .T. ) ;
#1116 = CARTESIAN_POINT ( 'NONE',  ( -40.34137639590981195, 34.12187500034139731, 29.30972558990012189 ) ) ;
#1117 = FACE_OUTER_BOUND ( 'NONE', #4619, .T. ) ;
#1118 = ORIENTED_EDGE ( 'NONE', *, *, #15652, .T. ) ;
#1119 = CIRCLE ( 'NONE', #15991, 50.00000000000000000 ) ;
#1120 = EDGE_CURVE ( 'NONE', #12156, #9153, #4935, .T. ) ;
#1121 = VERTEX_POINT ( 'NONE', #6248 ) ;
#1122 = CARTESIAN_POINT ( 'NONE',  ( 19.99999999999999289, 307.0000000000000568, -7.500000000000000000 ) ) ;
#1123 = CARTESIAN_POINT ( 'NONE',  ( 17.44929222242216227, 21.16875962481693207, 101.0000000000000000 ) ) ;
#1124 = CARTESIAN_POINT ( 'NONE',  ( -30.90169943749474513, 49.48125000068279178, -42.53254041760200721 ) ) ;
#1125 = DIRECTION ( 'NONE',  ( 0.000000000000000000, 0.000000000000000000, -1.000000000000000000 ) ) ;
#1126 = CARTESIAN_POINT ( 'NONE',  ( -30.81806926056962226, 30.15937500034139163, 42.41743335407647919 ) ) ;
#1127 =( NAMED_UNIT ( * ) SI_UNIT ( $, .STERADIAN. ) SOLID_ANGLE_UNIT ( ) );
#1128 = CARTESIAN_POINT ( 'NONE',  ( 49.86468353124999453, 47.02187500034139589, -16.20201782572376104 ) ) ;
#1129 = CARTESIAN_POINT ( 'NONE',  ( 0.000000000000000000, 0.000000000000000000, 0.000000000000000000 ) ) ;
#1130 = CARTESIAN_POINT ( 'NONE',  ( 4.320770838041294581, 30.97531352606685218, 101.0000000000000000 ) ) ;
#1131 = AXIS2_PLACEMENT_3D ( 'NONE', #1874, #6969, #10701 ) ;
#1132 = CARTESIAN_POINT ( 'NONE',  ( -50.00000000000000000, 35.78125000068280315, 0.000000000000000000 ) ) ;
#1133 =( NAMED_UNIT ( * ) PLANE_ANGLE_UNIT ( ) SI_UNIT ( $, .RADIAN. ) );
#1134 = ORIENTED_EDGE ( 'NONE', *, *, #1002, .F. ) ;
#1135 = CARTESIAN_POINT ( 'NONE',  ( -49.86468353125000164, 27.85937500034139447, 0.000000000000000000 ) ) ;
#1136 = CARTESIAN_POINT ( 'NONE',  ( -49.99999999999999289, 47.88125000068281167, 16.24598481164533226 ) ) ;
#1137 = ORIENTED_EDGE ( 'NONE', *, *, #2862, .T. ) ;
#1138 = VERTEX_POINT ( 'NONE', #14043 ) ;
#1139 = ADVANCED_FACE ( 'NONE', ( #16220 ), #10024, .T. ) ;
#1140 = CARTESIAN_POINT ( 'NONE',  ( -15.45084971874736368, 36.18125000068280173, 47.55282581475768211 ) ) ;
#1141 = LINE ( 'NONE', #8801, #3640 ) ;
#1142 = ADVANCED_FACE ( 'NONE', ( #7415 ), #13717, .T. ) ;
#1143 = DIRECTION ( 'NONE',  ( 0.000000000000000000, -0.7071067811865487940, 0.7071067811865463515 ) ) ;
#1145 = ORIENTED_EDGE ( 'NONE', *, *, #1475, .F. ) ;
#1144 = AXIS2_PLACEMENT_3D ( 'NONE', #13530, #1964, #3307 ) ;
#1146 = CARTESIAN_POINT ( 'NONE',  ( 40.45084971874737789, 38.58125000068280031, 29.38926261462365375 ) ) ;
#1147 = LINE ( 'NONE', #16290, #13270 ) ;
#1148 = CARTESIAN_POINT ( 'NONE',  ( 0.000000000000000000, 22.50000000000000000, 102.0000000000000142 ) ) ;
#1149 = CARTESIAN_POINT ( 'NONE',  ( 25.00000000000000000, 284.0710678118655323, 2.500000000000002220 ) ) ;
#1150 = CARTESIAN_POINT ( 'NONE',  ( -2.547328955960238000E-13, 32.28125000068278894, 49.99999999999999289 ) ) ;
#1151 = DIRECTION ( 'NONE',  ( 0.8660254037844432595, -0.4999999999999920064, 0.000000000000000000 ) ) ;
#1152 = DIRECTION ( 'NONE',  ( -0.000000000000000000, -1.000000000000000000, -0.000000000000000000 ) ) ;
#1153 = CARTESIAN_POINT ( 'NONE',  ( -30.90169943749473802, 46.08125000068278609, 42.53254041760200721 ) ) ;
#1154 =( BOUNDED_CURVE ( )  B_SPLINE_CURVE ( 3, ( #10835, #1003, #11172, #4860 ),
 .UNSPECIFIED., .F., .F. ) 
 B_SPLINE_CURVE_WITH_KNOTS ( ( 4, 4 ),
 ( 3.141592653589793116, 4.712388980384689674 ),
 .UNSPECIFIED. ) 
 CURVE ( )  GEOMETRIC_REPRESENTATION_ITEM ( )  RATIONAL_B_SPLINE_CURVE ( ( 1.000000000000000000, 0.8047378541243649375, 0.8047378541243649375, 1.000000000000000000 ) ) 
 REPRESENTATION_ITEM ( '' )  );
#1155 = FACE_OUTER_BOUND ( 'NONE', #4460, .T. ) ;
#1156 = CARTESIAN_POINT ( 'NONE',  ( 40.45084971874737079, 23.20000000000000284, -29.38926261462366440 ) ) ;
#1157 = CARTESIAN_POINT ( 'NONE',  ( -30.81806926056962226, 22.15937500034139873, 42.41743335407647919 ) ) ;
#1158 = CARTESIAN_POINT ( 'NONE',  ( -5.823736356558307894E-14, 44.50000000000000000, 50.00000000000000000 ) ) ;
#1159 = VECTOR ( 'NONE', #14041, 1000.000000000000000 ) ;
#1160 = CARTESIAN_POINT ( 'NONE',  ( -49.86468353124999453, 41.95937500034138878, 16.20201782572377525 ) ) ;
#1161 = EDGE_LOOP ( 'NONE', ( #1118, #2203, #12678, #13882 ) ) ;
#1162 = ORIENTED_EDGE ( 'NONE', *, *, #8619, .T. ) ;
#1163 = DIRECTION ( 'NONE',  ( 0.000000000000000000, 0.000000000000000000, 1.000000000000000000 ) ) ;
#1164 = CARTESIAN_POINT ( 'NONE',  ( -15.40903463028480580, 30.25937500034140015, 47.42413220539094709 ) ) ;
#1165 = EDGE_CURVE ( 'NONE', #5069, #10216, #1357, .T. ) ;
#1166 = EDGE_CURVE ( 'NONE', #13357, #14824, #3055, .T. ) ;
#1167 = DIRECTION ( 'NONE',  ( 0.000000000000000000, 0.000000000000000000, 1.000000000000000000 ) ) ;
#1168 = DIRECTION ( 'NONE',  ( 0.000000000000000000, 0.000000000000000000, -1.000000000000000000 ) ) ;
#1169 = CARTESIAN_POINT ( 'NONE',  ( 48.02615145421076193, 25.00000000000000000, -13.41652781627779234 ) ) ;
#1170 = AXIS2_PLACEMENT_3D ( 'NONE', #2365, #12760, #7448 ) ;
#1171 = CARTESIAN_POINT ( 'NONE',  ( 27.07106781186548261, 282.0000000000000000, -6.642135623730952787 ) ) ;
#1172 = CARTESIAN_POINT ( 'NONE',  ( -49.86468353124999453, 25.82187500034139305, -16.20201782572375393 ) ) ;
#1173 = CARTESIAN_POINT ( 'NONE',  ( -40.34137639590981905, 21.65937500034139518, -29.30972558990011478 ) ) ;
#1174 = CARTESIAN_POINT ( 'NONE',  ( 0.5000000000000000000, 244.0000000000000284, 49.99999999999999289 ) ) ;
#1175 = CARTESIAN_POINT ( 'NONE',  ( -15.40903463028480580, 34.32187500034139305, 47.42413220539094709 ) ) ;
#1176 = DIRECTION ( 'NONE',  ( 1.000000000000000000, 0.000000000000000000, 0.000000000000000000 ) ) ;
#1177 = CARTESIAN_POINT ( 'NONE',  ( 49.99999999999999289, 35.10000000000000853, -16.24598481164532160 ) ) ;
#1178 = CARTESIAN_POINT ( 'NONE',  ( 49.86468353125000164, 38.85937500034139447, -6.106662507704105588E-15 ) ) ;
#1179 = CARTESIAN_POINT ( 'NONE',  ( 49.86468353124999453, 29.02187500034139234, -16.20201782572376459 ) ) ;
#1180 = CARTESIAN_POINT ( 'NONE',  ( 50.00000000000000000, 43.00000000000000000, -6.123233995736766085E-15 ) ) ;
#1181 = VERTEX_POINT ( 'NONE', #2335 ) ;
#1182 = AXIS2_PLACEMENT_3D ( 'NONE', #5912, #10972, #15193 ) ;
#1183 = CARTESIAN_POINT ( 'NONE',  ( 30.81806926056964002, 34.55937500034139731, 42.41743335407646498 ) ) ;
#1184 = ORIENTED_EDGE ( 'NONE', *, *, #14174, .T. ) ;
#1185 = ORIENTED_EDGE ( 'NONE', *, *, #11085, .T. ) ;
#1186 = CARTESIAN_POINT ( 'NONE',  ( 15.45084971874736723, 23.18125000068279817, -47.55282581475768211 ) ) ;
#1187 = CARTESIAN_POINT ( 'NONE',  ( -49.99999999999999289, 33.89999999999999147, -16.24598481164531449 ) ) ;
#1188 = CARTESIAN_POINT ( 'NONE',  ( 9.631387414534489405E-15, 22.42187500034139802, 52.43083105670540789 ) ) ;
#1189 = DIRECTION ( 'NONE',  ( 0.000000000000000000, 1.000000000000000000, 0.000000000000000000 ) ) ;
#1190 = CARTESIAN_POINT ( 'NONE',  ( 30.81806926056964002, 42.62187500034139731, 42.41743335407647209 ) ) ;
#1191 = DIRECTION ( 'NONE',  ( 1.000000000000000000, -0.000000000000000000, 0.000000000000000000 ) ) ;
#1192 = AXIS2_PLACEMENT_3D ( 'NONE', #11874, #15769, #13204 ) ;
#1193 = CARTESIAN_POINT ( 'NONE',  ( -15.45084971874736368, 46.40000000000000568, 47.55282581475768211 ) ) ;
#1194 = CARTESIAN_POINT ( 'NONE',  ( 9.657523855033129090E-15, 30.28125000068279604, 52.57311121191334990 ) ) ;
#1195 = CARTESIAN_POINT ( 'NONE',  ( -30.81806926056963292, 49.62187500034139020, -42.41743335407647209 ) ) ;
#1196 = CARTESIAN_POINT ( 'NONE',  ( -30.81806926056963292, 35.62187500034140442, -42.41743335407647209 ) ) ;
#1197 = CARTESIAN_POINT ( 'NONE',  ( -24.86904120090709469, 286.8604097559688739, -7.369041200906229605 ) ) ;
#1198 = CARTESIAN_POINT ( 'NONE',  ( 15.40903463028482356, 38.52187500034139589, 47.42413220539093999 ) ) ;
#1199 = CARTESIAN_POINT ( 'NONE',  ( -5.000000000000000000, 96.75198296766780004, 7.580410092413951695 ) ) ;
#1200 = ORIENTED_EDGE ( 'NONE', *, *, #13732, .F. ) ;
#1201 = AXIS2_PLACEMENT_3D ( 'NONE', #11274, #16332, #1361 ) ;
#1202 = AXIS2_PLACEMENT_3D ( 'NONE', #5086, #7723, #7477 ) ;
#1203 = CIRCLE ( 'NONE', #13968, 42.00000000000000711 ) ;
#1204 = VECTOR ( 'NONE', #296, 1000.000000000000000 ) ;
#1205 = EDGE_CURVE ( 'NONE', #13562, #9978, #13349, .T. ) ;
#1206 = ORIENTED_EDGE ( 'NONE', *, *, #5813, .F. ) ;
#1207 = PRESENTATION_LAYER_ASSIGNMENT (  '', '', ( #11585 ) ) ;
#1208 = CARTESIAN_POINT ( 'NONE',  ( 1.486087262401875941, 13.10364194761998213, 101.0000000000000000 ) ) ;
#1209 = FACE_OUTER_BOUND ( 'NONE', #12628, .T. ) ;
#1210 = FACE_OUTER_BOUND ( 'NONE', #4894, .T. ) ;
#1211 = CARTESIAN_POINT ( 'NONE',  ( -48.35726954556750457, 20.00000000000000355, 12.16803787670978387 ) ) ;
#1212 = CARTESIAN_POINT ( 'NONE',  ( -30.81806926056963292, 33.55937500034138310, -42.41743335407647209 ) ) ;
#1213 = CARTESIAN_POINT ( 'NONE',  ( 5.000000000000000000, 121.6750890729884134, -29.67508907298829968 ) ) ;
#1214 = EDGE_CURVE ( 'NONE', #8474, #14735, #13959, .T. ) ;
#1215 = CARTESIAN_POINT ( 'NONE',  ( 30.81806926056964002, 46.62187500034139731, 42.41743335407646498 ) ) ;
#1216 =( LENGTH_UNIT ( ) NAMED_UNIT ( * ) SI_UNIT ( .MILLI., .METRE. ) );
#1217 = CIRCLE ( 'NONE', #4436, 50.00000000000000000 ) ;
#1218 = DIRECTION ( 'NONE',  ( 0.000000000000000000, 0.000000000000000000, -1.000000000000000000 ) ) ;
#1219 = CIRCLE ( 'NONE', #2556, 16.50000000000000711 ) ;
#1220 = DIRECTION ( 'NONE',  ( 0.8660254037844362651, 0.000000000000000000, -0.5000000000000041078 ) ) ;
#1221 = EDGE_CURVE ( 'NONE', #14428, #404, #5255, .T. ) ;
#1222 = DIRECTION ( 'NONE',  ( -0.000000000000000000, 0.000000000000000000, -1.000000000000000000 ) ) ;
#1223 = ORIENTED_EDGE ( 'NONE', *, *, #1722, .F. ) ;
#1224 = CARTESIAN_POINT ( 'NONE',  ( 40.34137639590981905, 22.65937500034139518, 29.30972558990010768 ) ) ;
#1225 = ORIENTED_EDGE ( 'NONE', *, *, #15661, .T. ) ;
#1226 = VERTEX_POINT ( 'NONE', #7814 ) ;
#1227 = ORIENTED_EDGE ( 'NONE', *, *, #9501, .T. ) ;
#1228 = VERTEX_POINT ( 'NONE', #484 ) ;
#1229 = EDGE_CURVE ( 'NONE', #8799, #14587, #16125, .T. ) ;
#1230 = AXIS2_PLACEMENT_3D ( 'NONE', #3697, #5194, #11341 ) ;
#1231 = FACE_OUTER_BOUND ( 'NONE', #5883, .T. ) ;
#1232 = DIRECTION ( 'NONE',  ( -0.000000000000000000, 0.7071067811865463515, 0.7071067811865487940 ) ) ;
#1233 = AXIS2_PLACEMENT_3D ( 'NONE', #15547, #11894, #4178 ) ;
#1234 =( NAMED_UNIT ( * ) SI_UNIT ( $, .STERADIAN. ) SOLID_ANGLE_UNIT ( ) );
#1235 = CARTESIAN_POINT ( 'NONE',  ( 1.293669679204937499E-13, 37.50000000000000711, -50.00000000000000000 ) ) ;
#1236 = CARTESIAN_POINT ( 'NONE',  ( 9.631387414534489405E-15, 48.35937500034140157, 52.43083105670540789 ) ) ;
#1237 = CARTESIAN_POINT ( 'NONE',  ( 0.000000000000000000, 22.50000000000000000, 102.0000000000000142 ) ) ;
#1238 = CARTESIAN_POINT ( 'NONE',  ( 30.90169943749475223, 26.48125000068279888, 42.53254041760199300 ) ) ;
#1239 = CARTESIAN_POINT ( 'NONE',  ( 0.000000000000000000, 22.50000000000000000, 102.0000000000000142 ) ) ;
#1240 = CYLINDRICAL_SURFACE ( 'NONE', #6816, 50.00000000000000000 ) ;
#1241 = CARTESIAN_POINT ( 'NONE',  ( 40.45084971874737079, 44.98125000068279888, -29.38926261462366440 ) ) ;
#1242 = CARTESIAN_POINT ( 'NONE',  ( -36.11321354817274454, 29.97008732934370911, 17.92868204048091840 ) ) ;
#1243 = CIRCLE ( 'NONE', #5001, 50.00000000000000000 ) ;
#1244 = CARTESIAN_POINT ( 'NONE',  ( 50.00000000000000711, 24.90000000000000213, 16.24598481164530739 ) ) ;
#1245 = CARTESIAN_POINT ( 'NONE',  ( 2.500000000000000000, 242.0000000000000284, -47.99999999999999289 ) ) ;
#1246 = DIRECTION ( 'NONE',  ( 0.000000000000000000, 0.000000000000000000, -1.000000000000000000 ) ) ;
#1247 = AXIS2_PLACEMENT_3D ( 'NONE', #12774, #6216, #11211 ) ;
#1248 = CARTESIAN_POINT ( 'NONE',  ( -3.210462471511496205E-15, 41.35937500034138736, -52.43083105670540789 ) ) ;
#1249 = EDGE_LOOP ( 'NONE', ( #3388, #224, #10891, #15269 ) ) ;
#1250 = EDGE_CURVE ( 'NONE', #9378, #8439, #5819, .T. ) ;
#1251 = CARTESIAN_POINT ( 'NONE',  ( 0.000000000000000000, 22.50000000000000000, 101.0000000000000000 ) ) ;
#1252 = ORIENTED_EDGE ( 'NONE', *, *, #15652, .F. ) ;
#1253 = DIRECTION ( 'NONE',  ( 1.000000000000000000, 0.000000000000000000, -2.312964634635742464E-16 ) ) ;
#1254 = CARTESIAN_POINT ( 'NONE',  ( 49.86468353125001585, 26.75937500034139660, 16.20201782572375038 ) ) ;
#1255 = AXIS2_PLACEMENT_3D ( 'NONE', #8224, #5420, #13290 ) ;
#1256 = DIRECTION ( 'NONE',  ( 0.000000000000000000, 0.000000000000000000, -1.000000000000000000 ) ) ;
#1257 = CARTESIAN_POINT ( 'NONE',  ( -15.72858266790894177, 30.19372578669147344, 93.36074974597489984 ) ) ;
#1258 = CARTESIAN_POINT ( 'NONE',  ( 47.88920767661677047, 25.00000000000000000, -13.89741811465768428 ) ) ;
#1259 = ADVANCED_BREP_SHAPE_REPRESENTATION ( '', ( #3161, #15812 ), #11844 ) ;
#1260 = CARTESIAN_POINT ( 'NONE',  ( -3.210462471511496205E-15, 37.42187500034140157, -52.43083105670540789 ) ) ;
#1261 =( BOUNDED_CURVE ( )  B_SPLINE_CURVE ( 2, ( #986, #7239, #9979, #6086, #8722, #5011, #13788, #12548, #1146, #3741, #8803, #13866, #7164 ),
 .UNSPECIFIED., .F., .F. ) 
 B_SPLINE_CURVE_WITH_KNOTS ( ( 3, 2, 2, 2, 2, 2, 3 ),
 ( 0.3500000000000000333, 0.3533333333333333326, 0.3599999999999999867, 0.3666666666666666408, 0.3733333333333333504, 0.3800000000000000044, 0.3833333333333333592 ),
 .UNSPECIFIED. ) 
 CURVE ( )  GEOMETRIC_REPRESENTATION_ITEM ( )  RATIONAL_B_SPLINE_CURVE ( ( 0.9755282581475768211, 0.9755282581475770431, 1.000000000000000000, 0.9510565162951535312, 1.000000000000000000, 0.9510565162951535312, 1.000000000000000000, 0.9510565162951535312, 1.000000000000000000, 0.9510565162951535312, 1.000000000000000000, 0.9755282581475765991, 0.9755282581475768211 ) ) 
 REPRESENTATION_ITEM ( '' )  );
#1262 = LINE ( 'NONE', #8827, #166 ) ;
#1263 = CARTESIAN_POINT ( 'NONE',  ( 30.81806926056962936, 25.15937500034139518, -42.41743335407646498 ) ) ;
#1264 = DIRECTION ( 'NONE',  ( 1.000000000000000000, 0.000000000000000000, 0.000000000000000000 ) ) ;
#1265 = CARTESIAN_POINT ( 'NONE',  ( 49.86468353125000164, 36.92187500034140157, -6.106662507704105588E-15 ) ) ;
#1266 = CARTESIAN_POINT ( 'NONE',  ( 0.000000000000000000, 22.50000000000000000, 101.0000000000000000 ) ) ;
#1267 = CARTESIAN_POINT ( 'NONE',  ( -49.99999999999999289, 33.90000000000000568, -16.24598481164531449 ) ) ;
#1268 = CARTESIAN_POINT ( 'NONE',  ( -15.40903463028481646, 39.45937500034139589, -47.42413220539093999 ) ) ;
#1269 = CARTESIAN_POINT ( 'NONE',  ( 40.34137639590981905, 32.72187500034139873, 29.30972558990010768 ) ) ;
#1270 = CARTESIAN_POINT ( 'NONE',  ( -50.00000000000000000, 46.00000000000000000, 0.000000000000000000 ) ) ;
#1271 = EDGE_CURVE ( 'NONE', #1479, #2396, #6753, .T. ) ;
#1272 = ORIENTED_EDGE ( 'NONE', *, *, #8288, .T. ) ;
#1273 = ORIENTED_EDGE ( 'NONE', *, *, #3682, .T. ) ;
#1274 = CARTESIAN_POINT ( 'NONE',  ( 30.81806926056962936, 35.15937500034139873, -42.41743335407646498 ) ) ;
#1275 = VERTEX_POINT ( 'NONE', #13128 ) ;
#1276 = ORIENTED_EDGE ( 'NONE', *, *, #15012, .T. ) ;
#1277 = CARTESIAN_POINT ( 'NONE',  ( 25.50583519765982743, 284.7842439685857698, -3.511670395308112536 ) ) ;
#1278 = CARTESIAN_POINT ( 'NONE',  ( -49.86468353124999453, 45.75937500034140015, -16.20201782572375393 ) ) ;
#1279 = CARTESIAN_POINT ( 'NONE',  ( 0.000000000000000000, 50.00000000000000000, 0.000000000000000000 ) ) ;
#1280 = CARTESIAN_POINT ( 'NONE',  ( 49.86468353125000164, 22.92187500034139802, -6.106662507704105588E-15 ) ) ;
#1281 = CYLINDRICAL_SURFACE ( 'NONE', #5229, 45.00000000000000711 ) ;
#1282 = CIRCLE ( 'NONE', #7664, 40.00000000000000000 ) ;
#1283 = CARTESIAN_POINT ( 'NONE',  ( 30.81806926056964002, 40.62187500034139731, 42.41743335407647209 ) ) ;
#1284 = CARTESIAN_POINT ( 'NONE',  ( -50.00000000000000000, 25.78125000068279959, 0.000000000000000000 ) ) ;
#1285 = CARTESIAN_POINT ( 'NONE',  ( 49.99999999999999289, 47.10000000000000853, -16.24598481164532160 ) ) ;
#1286 = CARTESIAN_POINT ( 'NONE',  ( -15.45084971874736368, 30.18125000068280173, 47.55282581475768211 ) ) ;
#1287 = CARTESIAN_POINT ( 'NONE',  ( 15.75363786119666720, 30.20531192536913423, 93.35498375726734821 ) ) ;
#1288 = CARTESIAN_POINT ( 'NONE',  ( -3.210462471511496205E-15, 37.42187500034140157, -52.43083105670540789 ) ) ;
#1289 = CARTESIAN_POINT ( 'NONE',  ( 50.00000000000000711, 38.89999999999999858, 16.24598481164530739 ) ) ;
#1290 = CARTESIAN_POINT ( 'NONE',  ( -49.99999999999999289, 27.89999999999999858, -16.24598481164531449 ) ) ;
#1291 = EDGE_LOOP ( 'NONE', ( #5186, #12830, #15543, #6502 ) ) ;
#1292 = ORIENTED_EDGE ( 'NONE', *, *, #6562, .F. ) ;
#1293 = DIRECTION ( 'NONE',  ( 0.5000000000000103251, -0.000000000000000000, 0.8660254037844328234 ) ) ;
#1294 = CARTESIAN_POINT ( 'NONE',  ( 7.500000000000000000, 25.00000000000000355, 39.29058411375427795 ) ) ;
#1295 = EDGE_CURVE ( 'NONE', #15320, #4877, #6671, .T. ) ;
#1296 = DIRECTION ( 'NONE',  ( 0.000000000000000000, 0.000000000000000000, -1.000000000000000000 ) ) ;
#1297 = EDGE_CURVE ( 'NONE', #4024, #14468, #9336, .T. ) ;
#1298 = CARTESIAN_POINT ( 'NONE',  ( -15.40903463028480580, 28.25937500034139660, 47.42413220539094709 ) ) ;
#1299 = CARTESIAN_POINT ( 'NONE',  ( 0.000000000000000000, 50.00000000000000000, 0.000000000000000000 ) ) ;
#1300 = CARTESIAN_POINT ( 'NONE',  ( 30.81806926056962936, 43.22187500034139873, -42.41743335407646498 ) ) ;
#1301 = FILL_AREA_STYLE ('',( #4995 ) ) ;
#1302 = DIRECTION ( 'NONE',  ( -0.000000000000000000, -1.000000000000000000, -0.000000000000000000 ) ) ;
#1303 = DIRECTION ( 'NONE',  ( 0.000000000000000000, 0.000000000000000000, 1.000000000000000000 ) ) ;
#1304 = DIRECTION ( 'NONE',  ( 0.000000000000000000, 0.000000000000000000, 1.000000000000000000 ) ) ;
#1305 = ORIENTED_EDGE ( 'NONE', *, *, #14153, .F. ) ;
#1306 = CARTESIAN_POINT ( 'NONE',  ( -15.40903463028480580, 22.25937500034139660, 47.42413220539094709 ) ) ;
#1307 = ORIENTED_EDGE ( 'NONE', *, *, #9049, .T. ) ;
#1308 = CARTESIAN_POINT ( 'NONE',  ( -30.90169943749473447, 46.08125000068279320, 42.53254041760200721 ) ) ;
#1309 = EDGE_CURVE ( 'NONE', #16149, #10856, #13257, .T. ) ;
#1310 = ORIENTED_EDGE ( 'NONE', *, *, #14892, .T. ) ;
#1311 = ORIENTED_EDGE ( 'NONE', *, *, #8778, .T. ) ;
#1312 = COLOUR_RGB ( '', 0.40784314, 0.44705882, 0.49803922) ;
#1313 = CARTESIAN_POINT ( 'NONE',  ( -49.86468353125000164, 49.85937500034139447, 0.000000000000000000 ) ) ;
#1314 = CARTESIAN_POINT ( 'NONE',  ( -2.547328955960238000E-13, 24.28125000068279604, 49.99999999999999289 ) ) ;
#1315 = CARTESIAN_POINT ( 'NONE',  ( -50.00000000000000000, 38.00000000000000711, 0.000000000000000000 ) ) ;
#1316 = CARTESIAN_POINT ( 'NONE',  ( 50.00000000000000711, 32.68125000068279462, 16.24598481164530739 ) ) ;
#1317 = FACE_OUTER_BOUND ( 'NONE', #13678, .T. ) ;
#1318 = CARTESIAN_POINT ( 'NONE',  ( -2.500000000000000000, 242.0000000000000284, 40.00000000000000000 ) ) ;
#1319 = CARTESIAN_POINT ( 'NONE',  ( 7.394441145214595501, 28.48516834767053751, 101.0000000000000000 ) ) ;
#1320 = FACE_OUTER_BOUND ( 'NONE', #15807, .T. ) ;
#1321 = CARTESIAN_POINT ( 'NONE',  ( 40.45084971874737789, 42.58125000068280031, 29.38926261462365375 ) ) ;
#1322 = DIRECTION ( 'NONE',  ( 0.000000000000000000, -1.000000000000000000, 0.000000000000000000 ) ) ;
#1323 = ADVANCED_FACE ( 'NONE', ( #11720 ), #1654, .T. ) ;
#1324 = CARTESIAN_POINT ( 'NONE',  ( -49.99999999999999289, 24.10000000000000142, 16.24598481164533226 ) ) ;
#1325 = CARTESIAN_POINT ( 'NONE',  ( 30.81806926056964002, 20.55937500034139376, 42.41743335407647209 ) ) ;
#1326 = VERTEX_POINT ( 'NONE', #11799 ) ;
#1327 = CARTESIAN_POINT ( 'NONE',  ( 9.631387414534489405E-15, 46.35937500034139447, 52.43083105670540789 ) ) ;
#1328 = VERTEX_POINT ( 'NONE', #9315 ) ;
#1329 = ADVANCED_FACE ( 'NONE', ( #5419 ), #15589, .T. ) ;
#1330 = PRESENTATION_STYLE_ASSIGNMENT (( #6175 ) ) ;
#1331 = CARTESIAN_POINT ( 'NONE',  ( -4.127528389677584286, 5.486372832567261604, 101.0000000000000000 ) ) ;
#1332 = CARTESIAN_POINT ( 'NONE',  ( -40.34137639590981195, 26.05937500034139731, 29.30972558990012189 ) ) ;
#1333 = ORIENTED_EDGE ( 'NONE', *, *, #14008, .T. ) ;
#1334 = EDGE_CURVE ( 'NONE', #13357, #2225, #2828, .T. ) ;
#1335 = PRODUCT_DEFINITION_SHAPE ( 'NONE', 'NONE',  #7215 ) ;
#1336 = CARTESIAN_POINT ( 'NONE',  ( -10.69075041230567891, 8.636095224584611429, 101.0000000000000000 ) ) ;
#1337 = CARTESIAN_POINT ( 'NONE',  ( -17.50000000000000000, 23.06298493376378289, 94.32371117417838491 ) ) ;
#1338 = CARTESIAN_POINT ( 'NONE',  ( 48.33688377893788157, 25.00000000000000000, -12.24883938693806229 ) ) ;
#1339 = CARTESIAN_POINT ( 'NONE',  ( -49.86468353125000164, 31.92187500034139447, 0.000000000000000000 ) ) ;
#1340 = CARTESIAN_POINT ( 'NONE',  ( 25.00000000000000000, 287.0000000000000568, -2.499999999999997780 ) ) ;
#1341 = CARTESIAN_POINT ( 'NONE',  ( -30.81806926056962226, 24.15937500034140228, 42.41743335407647209 ) ) ;
#1342 = LINE ( 'NONE', #2757, #2302 ) ;
#1343 = CARTESIAN_POINT ( 'NONE',  ( -49.86468353124999453, 33.82187500034138594, -16.20201782572375393 ) ) ;
#1344 = CYLINDRICAL_SURFACE ( 'NONE', #8409, 50.00000000000000000 ) ;
#1345 = CARTESIAN_POINT ( 'NONE',  ( -30.90169943749473802, 30.29999999999999716, 42.53254041760200721 ) ) ;
#1346 = CARTESIAN_POINT ( 'NONE',  ( -15.40903463028481646, 37.45937500034139589, -47.42413220539093999 ) ) ;
#1347 = CARTESIAN_POINT ( 'NONE',  ( -40.34137639590981905, 31.72187500034139873, -29.30972558990011478 ) ) ;
#1348 = CARTESIAN_POINT ( 'NONE',  ( 40.45084971874737789, 42.80000000000000426, 29.38926261462365375 ) ) ;
#1349 = ORIENTED_EDGE ( 'NONE', *, *, #2891, .T. ) ;
#1350 = ORIENTED_EDGE ( 'NONE', *, *, #10278, .F. ) ;
#1351 = CARTESIAN_POINT ( 'NONE',  ( -49.86468353125000164, 35.85937500034140157, 0.000000000000000000 ) ) ;
#1352 = VERTEX_POINT ( 'NONE', #9237 ) ;
#1353 = ORIENTED_EDGE ( 'NONE', *, *, #4912, .T. ) ;
#1354 = EDGE_CURVE ( 'NONE', #13340, #7372, #2628, .T. ) ;
#1355 = CARTESIAN_POINT ( 'NONE',  ( 23.39173249367926388, 283.2330659412876344, -9.195866246846929215 ) ) ;
#1357 =( BOUNDED_CURVE ( )  B_SPLINE_CURVE ( 2, ( #5176, #13798, #15047, #7569, #5020, #11320, #12645, #10232, #16298, #15291, #16386, #9909, #5097 ),
 .UNSPECIFIED., .F., .T. ) 
 B_SPLINE_CURVE_WITH_KNOTS ( ( 3, 2, 2, 2, 2, 2, 3 ),
 ( 0.9500000000000000666, 0.9533333333333333659, 0.9599999999999999645, 0.9666666666666666741, 0.9733333333333333837, 0.9799999999999999822, 0.9833333333333333925 ),
 .UNSPECIFIED. ) 
 CURVE ( )  GEOMETRIC_REPRESENTATION_ITEM ( )  RATIONAL_B_SPLINE_CURVE ( ( 0.9755282581475768211, 0.9755282581475771542, 1.000000000000000000, 0.9510565162951535312, 1.000000000000000000, 0.9510565162951535312, 1.000000000000000000, 0.9510565162951535312, 1.000000000000000000, 0.9510565162951535312, 1.000000000000000000, 0.9755282581475763770, 0.9755282581475768211 ) ) 
 REPRESENTATION_ITEM ( '' )  );
#1356 = CARTESIAN_POINT ( 'NONE',  ( -50.00000000000000000, 19.78125000068279604, 0.000000000000000000 ) ) ;
#1358 = EDGE_CURVE ( 'NONE', #11111, #10385, #14441, .T. ) ;
#1359 = DIRECTION ( 'NONE',  ( -0.000000000000000000, 1.000000000000000000, -0.000000000000000000 ) ) ;
#1360 = CARTESIAN_POINT ( 'NONE',  ( 49.86468353125000164, 20.92187500034139802, -6.106662507704105588E-15 ) ) ;
#1361 = DIRECTION ( 'NONE',  ( -1.000000000000000000, 0.000000000000000000, 0.000000000000000000 ) ) ;
#1362 = CARTESIAN_POINT ( 'NONE',  ( -15.40903463028480580, 44.32187500034140015, 47.42413220539094709 ) ) ;
#1363 = CARTESIAN_POINT ( 'NONE',  ( -15.40903463028481646, 45.45937500034139589, -47.42413220539093999 ) ) ;
#1364 = PLANE ( 'NONE',  #709 ) ;
#1365 = CARTESIAN_POINT ( 'NONE',  ( 15.45084971874737789, 46.60000000000000142, 47.55282581475767500 ) ) ;
#1366 = CARTESIAN_POINT ( 'NONE',  ( -49.99999999999999289, 29.88125000068279391, 16.24598481164533226 ) ) ;
#1367 = CARTESIAN_POINT ( 'NONE',  ( 10.69265510062280100, 36.36533908517922242, 92.97600696701006484 ) ) ;
#1368 = CARTESIAN_POINT ( 'NONE',  ( -49.86468353124999453, 32.02187500034139589, 16.20201782572377525 ) ) ;
#1369 = EDGE_CURVE ( 'NONE', #9016, #14108, #178, .T. ) ;
#1370 = CARTESIAN_POINT ( 'NONE',  ( 0.000000000000000000, 51.99999999999999289, 0.000000000000000000 ) ) ;
#1371 = EDGE_CURVE ( 'NONE', #15116, #12470, #2527, .T. ) ;
#1372 = ORIENTED_EDGE ( 'NONE', *, *, #7951, .F. ) ;
#1373 = ORIENTED_EDGE ( 'NONE', *, *, #5410, .T. ) ;
#1374 = DIRECTION ( 'NONE',  ( 0.8660254037844327124, 0.000000000000000000, -0.5000000000000102141 ) ) ;
#1375 = CARTESIAN_POINT ( 'NONE',  ( -22.35235477796478420, 99.04060251627524281, 5.000000000000000000 ) ) ;
#1376 = ADVANCED_FACE ( 'NONE', ( #9478 ), #8468, .F. ) ;
#1377 = CARTESIAN_POINT ( 'NONE',  ( -49.99999999999999289, 24.10000000000000142, 16.24598481164533226 ) ) ;
#1378 = DIRECTION ( 'NONE',  ( 0.000000000000000000, 0.000000000000000000, 1.000000000000000000 ) ) ;
#1379 = CARTESIAN_POINT ( 'NONE',  ( -49.86468353124999453, 33.75937500034140015, -16.20201782572375393 ) ) ;
#1380 = LINE ( 'NONE', #12700, #5056 ) ;
#1381 = CARTESIAN_POINT ( 'NONE',  ( 15.40903463028481113, 49.32187500034139305, -47.42413220539094709 ) ) ;
#1382 = CARTESIAN_POINT ( 'NONE',  ( 0.000000000000000000, 0.000000000000000000, 0.000000000000000000 ) ) ;
#1383 = CARTESIAN_POINT ( 'NONE',  ( 40.45084971874737789, 34.58125000068280031, 29.38926261462365375 ) ) ;
#1384 = LINE ( 'NONE', #16276, #6059 ) ;
#1385 = CARTESIAN_POINT ( 'NONE',  ( 0.000000000000000000, 52.00000000000000711, -60.00000000000000711 ) ) ;
#1386 = ORIENTED_EDGE ( 'NONE', *, *, #12039, .T. ) ;
#1387 = VECTOR ( 'NONE', #16201, 1000.000000000000000 ) ;
#1388 = CARTESIAN_POINT ( 'NONE',  ( -30.81806926056963292, 21.55937500034140086, -42.41743335407647209 ) ) ;
#1389 = ORIENTED_EDGE ( 'NONE', *, *, #1354, .F. ) ;
#1390 = CARTESIAN_POINT ( 'NONE',  ( -15.45084971874736368, 26.40000000000000213, 47.55282581475768211 ) ) ;
#1391 = ORIENTED_EDGE ( 'NONE', *, *, #564, .T. ) ;
#1392 = ORIENTED_EDGE ( 'NONE', *, *, #3028, .F. ) ;
#1393 = DIRECTION ( 'NONE',  ( -0.3090169943749573878, 0.9510565162951503115, 0.000000000000000000 ) ) ;
#1394 = CARTESIAN_POINT ( 'NONE',  ( 45.58196769024076644, 258.6644603543468861, -10.00000000000000178 ) ) ;
#1395 = CARTESIAN_POINT ( 'NONE',  ( -15.45084971874736368, 28.40000000000000213, 47.55282581475768211 ) ) ;
#1396 = DIRECTION ( 'NONE',  ( -0.7431448254773861395, -0.6691306063588672304, 0.000000000000000000 ) ) ;
#1397 = CARTESIAN_POINT ( 'NONE',  ( -3.210462471511496205E-15, 49.35937500034138736, -52.43083105670540789 ) ) ;
#1398 = DIRECTION ( 'NONE',  ( 0.8090169943749504489, -0.5877852522924689183, 0.000000000000000000 ) ) ;
#1399 = DIRECTION ( 'NONE',  ( 3.469446951953613696E-16, 0.000000000000000000, 1.000000000000000000 ) ) ;
#1400 = CARTESIAN_POINT ( 'NONE',  ( 30.90169943749475223, 24.48125000068279888, 42.53254041760199300 ) ) ;
#1401 = AXIS2_PLACEMENT_3D ( 'NONE', #13433, #9616, #10867 ) ;
#1402 = CARTESIAN_POINT ( 'NONE',  ( 0.000000000000000000, 267.0000000000000000, 0.000000000000000000 ) ) ;
#1403 = CARTESIAN_POINT ( 'NONE',  ( -3.219174618344376363E-15, 43.28125000068280315, -52.57311121191334990 ) ) ;
#1404 = CARTESIAN_POINT ( 'NONE',  ( 1.486087262401875941, 13.10364194761998213, 101.0000000000000000 ) ) ;
#1405 = CARTESIAN_POINT ( 'NONE',  ( 50.00000000000000000, 25.00000000000000000, -6.123233995736766085E-15 ) ) ;
#1406 = DIRECTION ( 'NONE',  ( -0.000000000000000000, -1.000000000000000000, -0.000000000000000000 ) ) ;
#1407 = VERTEX_POINT ( 'NONE', #4654 ) ;
#1408 = CARTESIAN_POINT ( 'NONE',  ( -15.40903463028480580, 38.25937500034140015, 47.42413220539094709 ) ) ;
#1409 = ORIENTED_EDGE ( 'NONE', *, *, #2371, .T. ) ;
#1410 = AXIS2_PLACEMENT_3D ( 'NONE', #16214, #14542, #13953 ) ;
#1411 = CARTESIAN_POINT ( 'NONE',  ( 40.45084971874737079, 42.98125000068279888, -29.38926261462366440 ) ) ;
#1412 = CARTESIAN_POINT ( 'NONE',  ( 0.000000000000000000, 22.50000000000000000, 102.0000000000000142 ) ) ;
#1413 = CARTESIAN_POINT ( 'NONE',  ( 40.34137639590981905, 30.65937500034139518, 29.30972558990010768 ) ) ;
#1414 = EDGE_CURVE ( 'NONE', #4999, #9634, #11090, .T. ) ;
#1415 = ORIENTED_EDGE ( 'NONE', *, *, #13921, .T. ) ;
#1416 = CARTESIAN_POINT ( 'NONE',  ( -2.547328955960238000E-13, 32.50000000000000000, 49.99999999999999289 ) ) ;
#1417 = DIRECTION ( 'NONE',  ( 0.000000000000000000, -1.000000000000000000, 0.000000000000000000 ) ) ;
#1418 = CARTESIAN_POINT ( 'NONE',  ( 47.39803307437463786, 25.00000000000000000, -15.49002591438228293 ) ) ;
#1419 = CARTESIAN_POINT ( 'NONE',  ( 15.40903463028481113, 37.32187500034140015, -47.42413220539094709 ) ) ;
#1420 = CARTESIAN_POINT ( 'NONE',  ( 7.919222016226807881, 46.33250428222964246, 50.00000000000000000 ) ) ;
#1421 = CARTESIAN_POINT ( 'NONE',  ( -15.40903463028480580, 22.25937500034139660, 47.42413220539094709 ) ) ;
#1422 = CARTESIAN_POINT ( 'NONE',  ( 1.034004556265705202E-14, 102.0000000000000142, 9.080892972013893782 ) ) ;
#1423 = CARTESIAN_POINT ( 'NONE',  ( 30.81806926056962936, 31.22187500034139518, -42.41743335407646498 ) ) ;
#1424 = EDGE_CURVE ( 'NONE', #4716, #8721, #4447, .T. ) ;
#1425 = CYLINDRICAL_SURFACE ( 'NONE', #14242, 5.000000000000000888 ) ;
#1427 = EDGE_CURVE ( 'NONE', #5069, #10576, #4749, .T. ) ;
#1426 = CIRCLE ( 'NONE', #12850, 40.00000000000000000 ) ;
#1428 = CARTESIAN_POINT ( 'NONE',  ( 40.45084971874737079, 29.19999999999999929, -29.38926261462366440 ) ) ;
#1429 = CARTESIAN_POINT ( 'NONE',  ( -49.86468353124999453, 31.95937500034139944, 16.20201782572377525 ) ) ;
#1430 = CARTESIAN_POINT ( 'NONE',  ( 40.34137639590981195, 31.12187500034139731, -29.30972558990011834 ) ) ;
#1431 = CARTESIAN_POINT ( 'NONE',  ( -3.219174618344376363E-15, 41.49999999999999289, -52.57311121191334990 ) ) ;
#1432 = EDGE_CURVE ( 'NONE', #8369, #9508, #559, .T. ) ;
#1433 = ORIENTED_EDGE ( 'NONE', *, *, #15400, .T. ) ;
#1434 = EDGE_CURVE ( 'NONE', #7069, #11084, #1969, .T. ) ;
#1435 = UNCERTAINTY_MEASURE_WITH_UNIT (LENGTH_MEASURE( 1.000000000000000082E-05 ), #1651, 'distance_accuracy_value', 'NONE');
#1436 = CARTESIAN_POINT ( 'NONE',  ( -30.81806926056962226, 36.15937500034139163, 42.41743335407647209 ) ) ;
#1437 = EDGE_LOOP ( 'NONE', ( #8797, #14710, #1373, #13540 ) ) ;
#1438 = ORIENTED_EDGE ( 'NONE', *, *, #16032, .F. ) ;
#1439 = CARTESIAN_POINT ( 'NONE',  ( 0.000000000000000000, 0.000000000000000000, 100.0000000000000000 ) ) ;
#1440 = CARTESIAN_POINT ( 'NONE',  ( -30.81806926056963292, 45.55937500034139731, -42.41743335407647209 ) ) ;
#1441 = AXIS2_PLACEMENT_3D ( 'NONE', #10549, #2890, #6473 ) ;
#1442 = DIRECTION ( 'NONE',  ( -0.000000000000000000, 1.000000000000000000, -0.000000000000000000 ) ) ;
#1443 = CARTESIAN_POINT ( 'NONE',  ( 40.34137639590981905, 24.72187500034139873, 29.30972558990010768 ) ) ;
#1444 = CARTESIAN_POINT ( 'NONE',  ( 9.574901606694759531E-15, 52.00000000000001421, -2.191293403013901479E-14 ) ) ;
#1445 = CARTESIAN_POINT ( 'NONE',  ( 15.40903463028481113, 35.32187500034139305, -47.42413220539094709 ) ) ;
#1446 = CARTESIAN_POINT ( 'NONE',  ( 49.86468353125000164, 40.85937500034139447, -6.106662507704105588E-15 ) ) ;
#1447 = CARTESIAN_POINT ( 'NONE',  ( 0.000000000000000000, 242.0000000000000284, -47.99999999999999289 ) ) ;
#1448 = CARTESIAN_POINT ( 'NONE',  ( -30.90169943749474868, 49.70000000000000284, -42.53254041760200721 ) ) ;
#1449 = CARTESIAN_POINT ( 'NONE',  ( 30.90169943749474157, 25.08125000068279675, -42.53254041760200721 ) ) ;
#1450 = CARTESIAN_POINT ( 'NONE',  ( 3.979171442067388931, 39.55125785365773083, 92.94260441222228053 ) ) ;
#1451 = AXIS2_PLACEMENT_3D ( 'NONE', #6325, #11391, #3740 ) ;
#1452 = CARTESIAN_POINT ( 'NONE',  ( -40.34137639590981195, 30.12187500034139731, 29.30972558990012189 ) ) ;
#1453 =( BOUNDED_CURVE ( )  B_SPLINE_CURVE ( 2, ( #4655, #4750, #9560, #12463, #7064, #9808, #12376, #14859, #3404, #9724, #13611, #6148, #14605 ),
 .UNSPECIFIED., .F., .F. ) 
 B_SPLINE_CURVE_WITH_KNOTS ( ( 3, 2, 2, 2, 2, 2, 3 ),
 ( 0.5166666666666667185, 0.5200000000000000178, 0.5266666666666666163, 0.5333333333333333259, 0.5400000000000000355, 0.5466666666666666341, 0.5500000000000000444 ),
 .UNSPECIFIED. ) 
 CURVE ( )  GEOMETRIC_REPRESENTATION_ITEM ( )  RATIONAL_B_SPLINE_CURVE ( ( 0.9755282581475768211, 0.9755282581475771542, 1.000000000000000000, 0.9510565162951535312, 1.000000000000000000, 0.9510565162951535312, 1.000000000000000000, 0.9510565162951535312, 1.000000000000000000, 0.9510565162951535312, 1.000000000000000000, 0.9755282581475763770, 0.9755282581475768211 ) ) 
 REPRESENTATION_ITEM ( '' )  );
#1454 = CARTESIAN_POINT ( 'NONE',  ( -0.5000000000000000000, 244.0000000000000284, 49.99999999999999289 ) ) ;
#1455 = ORIENTED_EDGE ( 'NONE', *, *, #11697, .T. ) ;
#1456 = CARTESIAN_POINT ( 'NONE',  ( -30.90169943749474868, 39.48125000068278467, -42.53254041760200721 ) ) ;
#1457 = ORIENTED_EDGE ( 'NONE', *, *, #8755, .F. ) ;
#1458 = VECTOR ( 'NONE', #4886, 999.9999999999998863 ) ;
#1459 = LINE ( 'NONE', #13398, #6549 ) ;
#1460 = DIRECTION ( 'NONE',  ( 0.000000000000000000, 0.7071067811865487940, -0.7071067811865463515 ) ) ;
#1461 = VECTOR ( 'NONE', #16017, 1000.000000000000000 ) ;
#1462 = CARTESIAN_POINT ( 'NONE',  ( -2.547328955960238000E-13, 24.49999999999999289, 49.99999999999999289 ) ) ;
#1463 = CARTESIAN_POINT ( 'NONE',  ( 15.40903463028481113, 49.32187500034139305, -47.42413220539094709 ) ) ;
#1464 = CARTESIAN_POINT ( 'NONE',  ( -15.40903463028481646, 31.45937500034139944, -47.42413220539093999 ) ) ;
#1465 = ADVANCED_BREP_SHAPE_REPRESENTATION ( '', ( #14144, #15812 ), #5488 ) ;
#1466 = LINE ( 'NONE', #4050, #4788 ) ;
#1467 = CARTESIAN_POINT ( 'NONE',  ( 30.81806926056962936, 47.22187500034139873, -42.41743335407646498 ) ) ;
#1468 = APPLICATION_PROTOCOL_DEFINITION ( 'draft international standard', 'automotive_design', 1998, #2490 ) ;
#1469 = CARTESIAN_POINT ( 'NONE',  ( 50.00000000000000000, 25.00000000000000000, -6.123233995736766085E-15 ) ) ;
#1470 = DIRECTION ( 'NONE',  ( 1.224646799147353207E-16, 1.000000000000000000, -0.000000000000000000 ) ) ;
#1471 = CARTESIAN_POINT ( 'NONE',  ( 8.660254037844387298, 20.00000000000000355, 5.000000000000000000 ) ) ;
#1472 = ORIENTED_EDGE ( 'NONE', *, *, #10992, .T. ) ;
#1473 = CIRCLE ( 'NONE', #15285, 5.000000000000000000 ) ;
#1474 = CARTESIAN_POINT ( 'NONE',  ( -30.81806926056962226, 46.22187500034139163, 42.41743335407647919 ) ) ;
#1475 = EDGE_CURVE ( 'NONE', #14428, #7907, #7062, .T. ) ;
#1476 = ORIENTED_EDGE ( 'NONE', *, *, #12004, .T. ) ;
#1477 = PLANE ( 'NONE',  #14226 ) ;
#1478 = EDGE_LOOP ( 'NONE', ( #4757, #9240, #1605, #15687, #2456, #2395, #11688, #12194 ) ) ;
#1479 = VERTEX_POINT ( 'NONE', #8774 ) ;
#1480 =( GEOMETRIC_REPRESENTATION_CONTEXT ( 3 ) GLOBAL_UNCERTAINTY_ASSIGNED_CONTEXT ( ( #6443 ) ) GLOBAL_UNIT_ASSIGNED_CONTEXT ( ( #5094, #4932, #3993 ) ) REPRESENTATION_CONTEXT ( 'NONE', 'WORKASPACE' ) );
#1481 = DIRECTION ( 'NONE',  ( -0.000000000000000000, -1.000000000000000000, -0.000000000000000000 ) ) ;
#1482 = CARTESIAN_POINT ( 'NONE',  ( 7.300484685132999196, 37.66786040234666189, 101.6666710451724214 ) ) ;
#1483 = CARTESIAN_POINT ( 'NONE',  ( -40.45084971874737079, 28.20000000000000284, 29.38926261462367151 ) ) ;
#1484 = CARTESIAN_POINT ( 'NONE',  ( -49.99999999999999289, 22.09999999999999787, 16.24598481164533226 ) ) ;
#1485 = VECTOR ( 'NONE', #16302, 1000.000000000000000 ) ;
#1486 = FACE_OUTER_BOUND ( 'NONE', #4355, .T. ) ;
#1487 = AXIS2_PLACEMENT_3D ( 'NONE', #7913, #11658, #14139 ) ;
#1488 = VECTOR ( 'NONE', #16400, 1000.000000000000000 ) ;
#1489 = CARTESIAN_POINT ( 'NONE',  ( 30.90169943749473802, 49.08125000068280031, -42.53254041760200721 ) ) ;
#1490 = CYLINDRICAL_SURFACE ( 'NONE', #7934, 40.00000000000000000 ) ;
#1491 = CIRCLE ( 'NONE', #5765, 40.00000000000000000 ) ;
#1492 = AXIS2_PLACEMENT_3D ( 'NONE', #15123, #13345, #9612 ) ;
#1493 = CARTESIAN_POINT ( 'NONE',  ( 40.34137639590981195, 25.12187500034139376, -29.30972558990011834 ) ) ;
#1494 =( GEOMETRIC_REPRESENTATION_CONTEXT ( 3 ) GLOBAL_UNCERTAINTY_ASSIGNED_CONTEXT ( ( #9092 ) ) GLOBAL_UNIT_ASSIGNED_CONTEXT ( ( #11140, #9883, #15945 ) ) REPRESENTATION_CONTEXT ( 'NONE', 'WORKASPACE' ) );
#1495 = DIRECTION ( 'NONE',  ( -0.3090169943749574988, 0.9510565162951503115, 0.000000000000000000 ) ) ;
#1496 = CARTESIAN_POINT ( 'NONE',  ( -40.45084971874737789, 39.58125000068280031, -29.38926261462365730 ) ) ;
#1497 = CARTESIAN_POINT ( 'NONE',  ( 15.83973438765496056, 27.12091057352781931, 102.0000000000000142 ) ) ;
#1498 = CARTESIAN_POINT ( 'NONE',  ( 7.919222016226827421, 47.22999571913595673, -50.00000000000000000 ) ) ;
#1499 = VERTEX_POINT ( 'NONE', #14772 ) ;
#1500 = CARTESIAN_POINT ( 'NONE',  ( 49.86468353125001585, 34.75937500034139305, 16.20201782572375038 ) ) ;
#1501 = ORIENTED_EDGE ( 'NONE', *, *, #1657, .T. ) ;
#1502 = VECTOR ( 'NONE', #1672, 999.9999999999998863 ) ;
#1503 = VECTOR ( 'NONE', #5732, 1000.000000000000227 ) ;
#1504 = AXIS2_PLACEMENT_3D ( 'NONE', #8311, #13377, #1981 ) ;
#1505 = CARTESIAN_POINT ( 'NONE',  ( 15.45084971874736723, 47.18125000068280173, -47.55282581475768211 ) ) ;
#1506 = DIRECTION ( 'NONE',  ( -0.000000000000000000, 1.000000000000000000, -0.000000000000000000 ) ) ;
#1507 = CARTESIAN_POINT ( 'NONE',  ( 30.81806926056964002, 30.55937500034139731, 42.41743335407647209 ) ) ;
#1508 = ORIENTED_EDGE ( 'NONE', *, *, #2739, .T. ) ;
#1509 = DIRECTION ( 'NONE',  ( 1.000000000000000000, 0.000000000000000000, -0.000000000000000000 ) ) ;
#1510 = CARTESIAN_POINT ( 'NONE',  ( -15.18866191491423479, 31.21127306749596642, 93.26832743753136867 ) ) ;
#1511 = LINE ( 'NONE', #10413, #67 ) ;
#1512 = CARTESIAN_POINT ( 'NONE',  ( -30.81806926056962226, 34.22187500034139163, 42.41743335407647209 ) ) ;
#1513 = EDGE_CURVE ( 'NONE', #326, #15172, #4405, .T. ) ;
#1514 = CARTESIAN_POINT ( 'NONE',  ( -49.99999999999999289, 29.68125000068279817, -16.24598481164531449 ) ) ;
#1515 = VECTOR ( 'NONE', #9722, 1000.000000000000000 ) ;
#1516 = CARTESIAN_POINT ( 'NONE',  ( -30.81806926056963292, 21.55937500034140086, -42.41743335407646498 ) ) ;
#1517 = CARTESIAN_POINT ( 'NONE',  ( -47.84248829804688086, 20.00000000000000355, 14.05740927763701187 ) ) ;
#1518 = CARTESIAN_POINT ( 'NONE',  ( -49.86468353124999453, 27.82187500034139305, -16.20201782572375393 ) ) ;
#1519 = AXIS2_PLACEMENT_3D ( 'NONE', #13845, #1293, #1374 ) ;
#1520 = CARTESIAN_POINT ( 'NONE',  ( -4.336808689942020818E-17, 307.0000000000000568, 2.500000000000001776 ) ) ;
#1521 = CARTESIAN_POINT ( 'NONE',  ( 30.90169943749474157, 33.30000000000000426, -42.53254041760200721 ) ) ;
#1522 = CARTESIAN_POINT ( 'NONE',  ( 15.40903463028481113, 29.25937500034139660, -47.42413220539094709 ) ) ;
#1523 = CARTESIAN_POINT ( 'NONE',  ( 15.40903463028481113, 29.32187500034139660, -47.42413220539094709 ) ) ;
#1524 = ADVANCED_FACE ( 'NONE', ( #5735 ), #9807, .T. ) ;
#1525 = ORIENTED_EDGE ( 'NONE', *, *, #1009, .T. ) ;
#1526 = CARTESIAN_POINT ( 'NONE',  ( 49.86468353125000164, 36.85937500034139447, -6.106662507704105588E-15 ) ) ;
#1527 = EDGE_CURVE ( 'NONE', #3819, #3901, #12127, .T. ) ;
#1528 = CARTESIAN_POINT ( 'NONE',  ( 26.02446187186532001, 283.9500510408986429, -4.548923743720680868 ) ) ;
#1529 = CARTESIAN_POINT ( 'NONE',  ( -49.86468353124999453, 47.95937500034138878, 16.20201782572377525 ) ) ;
#1530 = DIRECTION ( 'NONE',  ( -1.000000000000000000, -0.000000000000000000, -1.734723475976807094E-17 ) ) ;
#1531 = CARTESIAN_POINT ( 'NONE',  ( -15.40903463028481646, 23.52187500034139944, -47.42413220539093999 ) ) ;
#1532 = CARTESIAN_POINT ( 'NONE',  ( -26.23306594130729863, 283.6958662468272792, 4.966131882590584468 ) ) ;
#1533 = B_SPLINE_CURVE_WITH_KNOTS ( 'NONE', 3,
 ( #5559, #2707, #9037, #14261 ),
 .UNSPECIFIED., .F., .F.,
 ( 4, 4 ),
 ( 2.829004760673920638E-07, 0.001414802801989365486 ),
 .UNSPECIFIED. ) ;
#1534 = ADVANCED_FACE ( 'NONE', ( #5816, #3149 ), #10883, .T. ) ;
#1535 = CARTESIAN_POINT ( 'NONE',  ( -49.86468353124999453, 35.82187500034139305, -16.20201782572375393 ) ) ;
#1536 = CARTESIAN_POINT ( 'NONE',  ( -15.40903463028480580, 44.25937500034140015, 47.42413220539094709 ) ) ;
#1537 = LINE ( 'NONE', #6373, #11863 ) ;
#1538 = CARTESIAN_POINT ( 'NONE',  ( -40.34137639590981195, 20.12187500034139731, 29.30972558990012189 ) ) ;
#1539 = VECTOR ( 'NONE', #7143, 1000.000000000000000 ) ;
#1540 = CARTESIAN_POINT ( 'NONE',  ( 50.00000000000000711, 22.68125000068279462, 16.24598481164530739 ) ) ;
#1541 = CARTESIAN_POINT ( 'NONE',  ( 9.631387414534489405E-15, 48.42187500034140157, 52.43083105670540789 ) ) ;
#1542 = EDGE_CURVE ( 'NONE', #9634, #1788, #14255, .T. ) ;
#1543 = CARTESIAN_POINT ( 'NONE',  ( -40.34137639590981195, 28.12187500034139731, 29.30972558990012189 ) ) ;
#1544 = LINE ( 'NONE', #38, #15239 ) ;
#1545 = ORIENTED_EDGE ( 'NONE', *, *, #9863, .F. ) ;
#1546 = CARTESIAN_POINT ( 'NONE',  ( -30.90169943749474868, 35.48125000068279888, -42.53254041760200721 ) ) ;
#1547 = ORIENTED_EDGE ( 'NONE', *, *, #15147, .T. ) ;
#1548 = CARTESIAN_POINT ( 'NONE',  ( -13.22516817658079624, 40.70288237343621063, 101.0000000000000000 ) ) ;
#1549 = EDGE_CURVE ( 'NONE', #5607, #12984, #192, .T. ) ;
#1550 = CARTESIAN_POINT ( 'NONE',  ( -14.82166083077704499, 14.52006039870307852, 101.6666710451724214 ) ) ;
#1551 = CARTESIAN_POINT ( 'NONE',  ( 49.86468353124999453, 47.02187500034139589, -16.20201782572376104 ) ) ;
#1552 = CARTESIAN_POINT ( 'NONE',  ( 30.81806926056964002, 26.55937500034139376, 42.41743335407647209 ) ) ;
#1553 = CARTESIAN_POINT ( 'NONE',  ( 0.000000000000000000, 20.00000000000000355, 50.00000000000000000 ) ) ;
#1554 = CARTESIAN_POINT ( 'NONE',  ( 40.34137639590981195, 39.12187500034139731, -29.30972558990011834 ) ) ;
#1555 = CARTESIAN_POINT ( 'NONE',  ( 0.5000000000000000000, 245.0000000000000284, -49.99999999999999289 ) ) ;
#1556 = AXIS2_PLACEMENT_3D ( 'NONE', #10146, #14040, #6409 ) ;
#1557 = CARTESIAN_POINT ( 'NONE',  ( 49.86468353125000164, 44.92187500034140157, -6.106662507704105588E-15 ) ) ;
#1558 = FACE_OUTER_BOUND ( 'NONE', #10631, .T. ) ;
#1559 = ORIENTED_EDGE ( 'NONE', *, *, #4297, .F. ) ;
#1560 = CARTESIAN_POINT ( 'NONE',  ( -3.210462471511496205E-15, 49.42187500034138736, -52.43083105670540789 ) ) ;
#1561 = ORIENTED_EDGE ( 'NONE', *, *, #11744, .T. ) ;
#1562 = CARTESIAN_POINT ( 'NONE',  ( -0.5000000000000000000, 39.65938208326293335, 101.3333374618097480 ) ) ;
#1563 = EDGE_LOOP ( 'NONE', ( #13749, #13457, #3721, #959 ) ) ;
#1564 = ORIENTED_EDGE ( 'NONE', *, *, #1250, .T. ) ;
#1565 = EDGE_CURVE ( 'NONE', #3318, #383, #2418, .T. ) ;
#1566 = CARTESIAN_POINT ( 'NONE',  ( -49.99999999999999289, 43.68125000068280173, -16.24598481164531449 ) ) ;
#1567 = DIRECTION ( 'NONE',  ( -0.000000000000000000, 0.7071067811865463515, 0.7071067811865487940 ) ) ;
#1568 = CARTESIAN_POINT ( 'NONE',  ( 15.45084971874736723, 29.40000000000000213, -47.55282581475768211 ) ) ;
#1569 = CARTESIAN_POINT ( 'NONE',  ( -30.90169943749474868, 27.70000000000000284, -42.53254041760200721 ) ) ;
#1570 = VECTOR ( 'NONE', #9716, 1000.000000000000114 ) ;
#1571 = CARTESIAN_POINT ( 'NONE',  ( -49.86468353124999453, 45.75937500034140015, -16.20201782572375393 ) ) ;
#1572 = DIRECTION ( 'NONE',  ( 0.000000000000000000, -1.000000000000000000, 0.000000000000000000 ) ) ;
#1573 = DIRECTION ( 'NONE',  ( -0.000000000000000000, -0.000000000000000000, 1.000000000000000000 ) ) ;
#1574 = CARTESIAN_POINT ( 'NONE',  ( 49.86468353124999453, 21.02187500034139589, -16.20201782572376459 ) ) ;
#1575 =( LENGTH_UNIT ( ) NAMED_UNIT ( * ) SI_UNIT ( .MILLI., .METRE. ) );
#1576 = CARTESIAN_POINT ( 'NONE',  ( 0.000000000000000000, 272.0000000000000000, 0.000000000000000000 ) ) ;
#1577 = CARTESIAN_POINT ( 'NONE',  ( 40.45084971874737079, 42.98125000068279888, -29.38926261462366440 ) ) ;
#1578 = CARTESIAN_POINT ( 'NONE',  ( -7.919222016226822092, 46.44874571845315359, 50.00000000000000000 ) ) ;
#1579 = CARTESIAN_POINT ( 'NONE',  ( -17.28626291527383785, 25.00000000000000355, 18.64048258526051427 ) ) ;
#1580 = DIRECTION ( 'NONE',  ( -0.000000000000000000, -1.000000000000000000, -0.000000000000000000 ) ) ;
#1581 = ORIENTED_EDGE ( 'NONE', *, *, #8035, .T. ) ;
#1582 = CARTESIAN_POINT ( 'NONE',  ( 49.86468353124999453, 36.95937500034139589, -16.20201782572376459 ) ) ;
#1583 = AXIS2_PLACEMENT_3D ( 'NONE', #310, #15194, #13947 ) ;
#1584 = ORIENTED_EDGE ( 'NONE', *, *, #1798, .F. ) ;
#1585 = CARTESIAN_POINT ( 'NONE',  ( 30.90169943749475578, 48.48125000068279888, 42.53254041760200010 ) ) ;
#1586 = CARTESIAN_POINT ( 'NONE',  ( 8.446640517145639571E-15, 28.49999999999999645, 50.00000000000000000 ) ) ;
#1587 = CARTESIAN_POINT ( 'NONE',  ( 49.86468353124999453, 20.95937500034138878, -16.20201782572376459 ) ) ;
#1588 = ORIENTED_EDGE ( 'NONE', *, *, #13663, .F. ) ;
#1589 = CARTESIAN_POINT ( 'NONE',  ( 7.919222016226809657, 27.44874571845315003, -50.00000000000000000 ) ) ;
#1590 = CARTESIAN_POINT ( 'NONE',  ( -13.21908673885165086, 34.02500059410989763, 93.06976900205165748 ) ) ;
#1591 = DIRECTION ( 'NONE',  ( 0.000000000000000000, -1.000000000000000000, 0.000000000000000000 ) ) ;
#1592 = CARTESIAN_POINT ( 'NONE',  ( -30.81806926056962226, 28.22187500034139873, 42.41743335407647209 ) ) ;
#1593 = CARTESIAN_POINT ( 'NONE',  ( 0.000000000000000000, 22.50000000000000000, 102.0000000000000142 ) ) ;
#1594 = CARTESIAN_POINT ( 'NONE',  ( 17.47157445415547983, 21.34957311187938700, 94.63625203854948609 ) ) ;
#1595 = CARTESIAN_POINT ( 'NONE',  ( -46.68017951973648394, 20.00000000000001066, 17.53418100958496595 ) ) ;
#1596 = CARTESIAN_POINT ( 'NONE',  ( -3.210462471511496205E-15, 29.42187500034139447, -52.43083105670540789 ) ) ;
#1597 = CARTESIAN_POINT ( 'NONE',  ( -49.99999999999999289, 21.90000000000000213, -16.24598481164531449 ) ) ;
#1598 = CARTESIAN_POINT ( 'NONE',  ( -50.00000000000000000, 36.00000000000000711, 0.000000000000000000 ) ) ;
#1599 = CARTESIAN_POINT ( 'NONE',  ( 49.86468353125000164, 32.85937500034139447, -6.106662507704105588E-15 ) ) ;
#1600 = CARTESIAN_POINT ( 'NONE',  ( 30.81806926056962936, 27.22187500034139518, -42.41743335407647209 ) ) ;
#1601 = FACE_OUTER_BOUND ( 'NONE', #8159, .T. ) ;
#1602 = VERTEX_POINT ( 'NONE', #202 ) ;
#1603 =( BOUNDED_SURFACE ( )  B_SPLINE_SURFACE ( 3, 2, ( 
 ( #6296, #4813, #7207 ),
 ( #11029, #3384, #2287 ),
 ( #8777, #13760, #10038 ),
 ( #3547, #9866, #14751 ),
 ( #16098, #4732, #7532 ),
 ( #8600, #11365, #8524 ),
 ( #13514, #7379, #12445 ),
 ( #1036, #13839, #12523 ),
 ( #2198, #12268, #7456 ),
 ( #870, #2453, #11204 ),
 ( #7295, #952, #15002 ),
 ( #9790, #11123, #5966 ),
 ( #12603, #12351, #16256 ),
 ( #6053, #4890, #9947 ),
 ( #3638, #1197, #8694 ),
 ( #2373, #1114, #16432 ),
 ( #6210, #11281, #12998 ),
 ( #4101, #11444, #10425 ) ),
 .UNSPECIFIED., .F., .F., .F. ) 
 B_SPLINE_SURFACE_WITH_KNOTS ( ( 4, 2, 2, 2, 2, 2, 2, 2, 4 ),
 ( 3, 3 ),
 ( 1.570796326794896558, 1.767145867644258628, 1.963495408493620697, 2.159844949342982545, 2.356194490192344837, 2.552544031041707129, 2.748893571891068976, 2.945243112740430824, 3.141592653589793116 ),
 ( 0.000000000000000000, 1.000000000000000000 ),
 .UNSPECIFIED. ) 
 GEOMETRIC_REPRESENTATION_ITEM ( )  RATIONAL_B_SPLINE_SURFACE ( (
 ( 1.000000000000000000, 1.000000000000000000, 1.000000000000000000),
 ( 1.000000000000000000, 1.000000000000000000, 1.000000000000000000),
 ( 1.000000000000000000, 0.9967613244521498217, 1.000000000000000000),
 ( 1.000000000000000000, 0.9841171504955907867, 1.000000000000000000),
 ( 1.000000000000000000, 0.9747108043452232806, 1.000000000000000000),
 ( 1.000000000000000000, 0.9506740354170890583, 1.000000000000000000),
 ( 1.000000000000000000, 0.9360421842396997594, 1.000000000000000000),
 ( 1.000000000000000000, 0.9031650994466968729, 1.000000000000000000),
 ( 1.000000000000000000, 0.8849191470854506081, 1.000000000000000000),
 ( 1.000000000000000000, 0.8471316604834270292, 1.000000000000000000),
 ( 1.000000000000000000, 0.8275942695279743244, 1.000000000000000000),
 ( 1.000000000000000000, 0.7902180087153679588, 1.000000000000000000),
 ( 1.000000000000000000, 0.7723968217385259738, 1.000000000000000000),
 ( 1.000000000000000000, 0.7418334179586800747, 1.000000000000000000),
 ( 1.000000000000000000, 0.7291288939600593100, 1.000000000000000000),
 ( 1.000000000000000000, 0.7117460025832584858, 1.000000000000000000),
 ( 1.000000000000000000, 0.7070717283367141670, 1.000000000000000000),
 ( 1.000000000000000000, 0.7071067811865475727, 1.000000000000000000) ) ) 
 REPRESENTATION_ITEM ( '' )  SURFACE ( )  );
#1604 = CARTESIAN_POINT ( 'NONE',  ( 30.81806926056962936, 27.15937500034139163, -42.41743335407646498 ) ) ;
#1605 = ORIENTED_EDGE ( 'NONE', *, *, #9196, .T. ) ;
#1606 = CARTESIAN_POINT ( 'NONE',  ( 21.32168401022778070, 284.4942466289054437, -8.160842005109239850 ) ) ;
#1607 = CARTESIAN_POINT ( 'NONE',  ( -30.81806926056963292, 43.55937500034139731, -42.41743335407647209 ) ) ;
#1608 = DIRECTION ( 'NONE',  ( 0.000000000000000000, 0.000000000000000000, 1.000000000000000000 ) ) ;
#1609 = FACE_OUTER_BOUND ( 'NONE', #8042, .T. ) ;
#1610 = CARTESIAN_POINT ( 'NONE',  ( -26.77784341583514305, 282.2553694771637538, 10.88892170791705283 ) ) ;
#1611 = CARTESIAN_POINT ( 'NONE',  ( -49.86468353125000164, 35.92187500034140157, 0.000000000000000000 ) ) ;
#1612 = CARTESIAN_POINT ( 'NONE',  ( -49.86468353124999453, 37.95937500034139589, 16.20201782572377169 ) ) ;
#1613 = CARTESIAN_POINT ( 'NONE',  ( 0.000000000000000000, 262.0000000000000000, 0.000000000000000000 ) ) ;
#1614 = CARTESIAN_POINT ( 'NONE',  ( -40.45084971874737079, 38.20000000000000284, 29.38926261462367151 ) ) ;
#1615 = PRODUCT_DEFINITION_SHAPE ( 'NONE', 'NONE',  #14821 ) ;
#1616 = CARTESIAN_POINT ( 'NONE',  ( -30.81806926056963292, 49.55937500034139731, -42.41743335407647209 ) ) ;
#1617 = CARTESIAN_POINT ( 'NONE',  ( 49.86468353125001585, 46.82187500034139305, 16.20201782572375038 ) ) ;
#1618 = CARTESIAN_POINT ( 'NONE',  ( 49.86468353124999453, 31.02187500034139234, -16.20201782572376459 ) ) ;
#1619 = CARTESIAN_POINT ( 'NONE',  ( -49.86468353125000164, 47.85937500034139447, 0.000000000000000000 ) ) ;
#1620 = ORIENTED_EDGE ( 'NONE', *, *, #4694, .T. ) ;
#1621 = CARTESIAN_POINT ( 'NONE',  ( 9.657523855033129090E-15, 34.28125000068278894, 52.57311121191334990 ) ) ;
#1622 = EDGE_LOOP ( 'NONE', ( #5422, #797, #7323, #9730 ) ) ;
#1623 = CARTESIAN_POINT ( 'NONE',  ( 0.000000000000000000, 20.00000000000000355, 0.000000000000000000 ) ) ;
#1624 = CARTESIAN_POINT ( 'NONE',  ( 0.000000000000000000, 272.0000000000000000, -82.49773270518484480 ) ) ;
#1625 = EDGE_CURVE ( 'NONE', #3391, #14186, #2782, .T. ) ;
#1626 = CARTESIAN_POINT ( 'NONE',  ( 50.00000000000000000, 32.78125000068279604, -6.123233995736766085E-15 ) ) ;
#1627 = CARTESIAN_POINT ( 'NONE',  ( 49.86468353125001585, 44.82187500034139305, 16.20201782572375038 ) ) ;
#1628 = CARTESIAN_POINT ( 'NONE',  ( 15.40903463028482356, 24.45937500034139589, 47.42413220539093999 ) ) ;
#1629 = CARTESIAN_POINT ( 'NONE',  ( -30.90169943749474513, 39.48125000068278467, -42.53254041760200721 ) ) ;
#1630 = CARTESIAN_POINT ( 'NONE',  ( -49.86468353125000164, 41.92187500034139447, 0.000000000000000000 ) ) ;
#1631 = FACE_OUTER_BOUND ( 'NONE', #14650, .T. ) ;
#1632 = ADVANCED_FACE ( 'NONE', ( #12769 ), #7108, .T. ) ;
#1633 = EDGE_CURVE ( 'NONE', #2064, #9033, #3918, .T. ) ;
#1634 = CARTESIAN_POINT ( 'NONE',  ( 15.40903463028481113, 45.32187500034140015, -47.42413220539094709 ) ) ;
#1635 = CARTESIAN_POINT ( 'NONE',  ( -6.725310538855818976, 29.22831317314782851, 101.0000000000000000 ) ) ;
#1636 = ORIENTED_EDGE ( 'NONE', *, *, #16217, .T. ) ;
#1637 = EDGE_CURVE ( 'NONE', #8883, #15854, #7499, .T. ) ;
#1638 = CARTESIAN_POINT ( 'NONE',  ( 30.81806926056964002, 48.62187500034139731, 42.41743335407647209 ) ) ;
#1639 = VERTEX_POINT ( 'NONE', #1891 ) ;
#1640 = CARTESIAN_POINT ( 'NONE',  ( -7.919222016226804328, 26.44874571845315359, 50.00000000000000000 ) ) ;
#1641 = VERTEX_POINT ( 'NONE', #2989 ) ;
#1642 = ORIENTED_EDGE ( 'NONE', *, *, #3754, .T. ) ;
#1643 = CARTESIAN_POINT ( 'NONE',  ( -5.823736356558307894E-14, 44.28125000068280315, 50.00000000000000000 ) ) ;
#1644 = CARTESIAN_POINT ( 'NONE',  ( 22.35235477796478420, 99.04060251627522860, -5.000000000000000000 ) ) ;
#1645 = LINE ( 'NONE', #10562, #16454 ) ;
#1646 = CARTESIAN_POINT ( 'NONE',  ( 50.00000000000000000, 23.00000000000000355, -6.123233995736766085E-15 ) ) ;
#1647 = CARTESIAN_POINT ( 'NONE',  ( -30.81806926056963292, 41.55937500034139731, -42.41743335407647209 ) ) ;
#1648 = CARTESIAN_POINT ( 'NONE',  ( -50.00000000000000000, 25.78125000068279959, 0.000000000000000000 ) ) ;
#1649 = DIRECTION ( 'NONE',  ( -0.000000000000000000, -1.000000000000000000, -0.000000000000000000 ) ) ;
#1650 = CARTESIAN_POINT ( 'NONE',  ( -30.90169943749473447, 46.30000000000000426, 42.53254041760200721 ) ) ;
#1651 =( LENGTH_UNIT ( ) NAMED_UNIT ( * ) SI_UNIT ( .MILLI., .METRE. ) );
#1652 = CARTESIAN_POINT ( 'NONE',  ( -3.111920190527341144E-15, 43.28125000068280315, -50.00000000000000000 ) ) ;
#1653 = CARTESIAN_POINT ( 'NONE',  ( 15.45084971874736723, 43.18125000068280173, -47.55282581475768211 ) ) ;
#1654 = CYLINDRICAL_SURFACE ( 'NONE', #4727, 2.000000000000001776 ) ;
#1655 = AXIS2_PLACEMENT_3D ( 'NONE', #14370, #1406, #6837 ) ;
#1656 = FACE_OUTER_BOUND ( 'NONE', #3657, .T. ) ;
#1657 = EDGE_CURVE ( 'NONE', #2087, #5830, #2424, .T. ) ;
#1658 = VERTEX_POINT ( 'NONE', #1579 ) ;
#1659 = CARTESIAN_POINT ( 'NONE',  ( 49.86468353125000164, 36.85937500034139447, -6.106662507704105588E-15 ) ) ;
#1660 = ORIENTED_EDGE ( 'NONE', *, *, #5200, .T. ) ;
#1661 = ORIENTED_EDGE ( 'NONE', *, *, #2650, .F. ) ;
#1662 = ADVANCED_FACE ( 'NONE', ( #1656 ), #485, .T. ) ;
#1663 = DIRECTION ( 'NONE',  ( 0.000000000000000000, 1.000000000000000000, 0.000000000000000000 ) ) ;
#1664 = CARTESIAN_POINT ( 'NONE',  ( 0.000000000000000000, 25.00000000000000355, 0.000000000000000000 ) ) ;
#1665 = CARTESIAN_POINT ( 'NONE',  ( -49.86468353124999453, 19.95937500034138878, 16.20201782572377525 ) ) ;
#1667 = ORIENTED_EDGE ( 'NONE', *, *, #11380, .T. ) ;
#1666 = VECTOR ( 'NONE', #3718, 1000.000000000000000 ) ;
#1668 = CARTESIAN_POINT ( 'NONE',  ( 0.000000000000000000, 252.1309828287255357, 0.000000000000000000 ) ) ;
#1669 = CARTESIAN_POINT ( 'NONE',  ( 15.45084971874736723, 35.39999999999999858, -47.55282581475768211 ) ) ;
#1670 = DIRECTION ( 'NONE',  ( -0.5000000000000042188, 0.000000000000000000, -0.8660254037844362651 ) ) ;
#1671 = CARTESIAN_POINT ( 'NONE',  ( 49.86468353124999453, 29.02187500034139234, -16.20201782572376104 ) ) ;
#1672 = DIRECTION ( 'NONE',  ( -0.8660254037844361541, 0.000000000000000000, 0.5000000000000043299 ) ) ;
#1673 = CARTESIAN_POINT ( 'NONE',  ( 15.45084971874736723, 47.40000000000000568, -47.55282581475768211 ) ) ;
#1674 = CARTESIAN_POINT ( 'NONE',  ( 5.988468393966018155, 15.10823117958429584, 101.0000000000000000 ) ) ;
#1675 = CARTESIAN_POINT ( 'NONE',  ( -30.81806926056963292, 31.62187500034140086, -42.41743335407646498 ) ) ;
#1676 = CARTESIAN_POINT ( 'NONE',  ( -2.464234863135557063, 13.31155363843772932, 102.0000000000000142 ) ) ;
#1677 = CARTESIAN_POINT ( 'NONE',  ( 30.90169943749474157, 37.30000000000000426, -42.53254041760200721 ) ) ;
#1678 = CARTESIAN_POINT ( 'NONE',  ( -40.34137639590981905, 29.65937500034139518, -29.30972558990011478 ) ) ;
#1679 = AXIS2_PLACEMENT_3D ( 'NONE', #3745, #10067, #1399 ) ;
#1680 = CARTESIAN_POINT ( 'NONE',  ( 7.919222016226758143, 38.55125428154684641, 50.00000000000000711 ) ) ;
#1681 = ORIENTED_EDGE ( 'NONE', *, *, #11408, .T. ) ;
#1682 = EDGE_CURVE ( 'NONE', #10619, #5249, #15486, .T. ) ;
#1683 = CARTESIAN_POINT ( 'NONE',  ( -3.210462471511496205E-15, 31.35937500034138736, -52.43083105670540789 ) ) ;
#1684 = EDGE_CURVE ( 'NONE', #8698, #14922, #1243, .T. ) ;
#1685 = ORIENTED_EDGE ( 'NONE', *, *, #6952, .T. ) ;
#1686 = DIRECTION ( 'NONE',  ( -1.000000000000000000, 0.000000000000000000, 0.000000000000000000 ) ) ;
#1687 = CARTESIAN_POINT ( 'NONE',  ( -49.86468353125000164, 43.85937500034140157, 0.000000000000000000 ) ) ;
#1688 = CARTESIAN_POINT ( 'NONE',  ( 5.849792707072439590, 106.0483007247212015, 5.000000000000000888 ) ) ;
#1689 = CARTESIAN_POINT ( 'NONE',  ( 24.96465690379361035, 286.9981936728412393, 7.464656903795364506 ) ) ;
#1690 = AXIS2_PLACEMENT_3D ( 'NONE', #3485, #4748, #13609 ) ;
#1691 = CARTESIAN_POINT ( 'NONE',  ( -20.31983351293596129, 285.7035871579731179, 7.659916756467385568 ) ) ;
#1692 = CARTESIAN_POINT ( 'NONE',  ( 49.86468353125000164, 32.92187500034139447, -6.106662507704105588E-15 ) ) ;
#1693 = CARTESIAN_POINT ( 'NONE',  ( -15.40903463028480580, 36.25937500034140015, 47.42413220539094709 ) ) ;
#1694 = CARTESIAN_POINT ( 'NONE',  ( -3.111920190527341144E-15, 25.50000000000000355, -50.00000000000000000 ) ) ;
#1695 = CARTESIAN_POINT ( 'NONE',  ( -40.45084971874737079, 42.20000000000000284, 29.38926261462367151 ) ) ;
#1696 = CARTESIAN_POINT ( 'NONE',  ( 49.99999999999999289, 22.88125000068280102, -16.24598481164532160 ) ) ;
#1697 = CARTESIAN_POINT ( 'NONE',  ( 49.86468353125000164, 42.92187500034140157, -6.106662507704105588E-15 ) ) ;
#1698 =( BOUNDED_CURVE ( )  B_SPLINE_CURVE ( 2, ( #7324, #12395, #4842, #4667, #14870, #8635, #5996, #13547, #12299, #13623, #16135, #10975, #901 ),
 .UNSPECIFIED., .F., .F. ) 
 B_SPLINE_CURVE_WITH_KNOTS ( ( 3, 2, 2, 2, 2, 2, 3 ),
 ( 0.05000000000000000278, 0.05333333333333333676, 0.05999999999999999778, 0.06666666666666666574, 0.07333333333333333370, 0.08000000000000000167, 0.08333333333333334259 ),
 .UNSPECIFIED. ) 
 CURVE ( )  GEOMETRIC_REPRESENTATION_ITEM ( )  RATIONAL_B_SPLINE_CURVE ( ( 0.9755282581475768211, 0.9755282581475768211, 1.000000000000000000, 0.9510565162951535312, 1.000000000000000000, 0.9510565162951535312, 1.000000000000000000, 0.9510565162951535312, 1.000000000000000000, 0.9510565162951535312, 1.000000000000000000, 0.9755282581475767101, 0.9755282581475768211 ) ) 
 REPRESENTATION_ITEM ( '' )  );
#1699 = CARTESIAN_POINT ( 'NONE',  ( -49.86468353125000164, 25.92187500034139802, 0.000000000000000000 ) ) ;
#1700 = VECTOR ( 'NONE', #10071, 1000.000000000000000 ) ;
#1701 = CARTESIAN_POINT ( 'NONE',  ( -7.919222016226816763, 27.33250428222964246, -49.99999999999999289 ) ) ;
#1702 = ORIENTED_EDGE ( 'NONE', *, *, #5817, .F. ) ;
#1703 = CARTESIAN_POINT ( 'NONE',  ( -30.90169943749474868, 33.48125000068279888, -42.53254041760200721 ) ) ;
#1704 = EDGE_LOOP ( 'NONE', ( #4465, #8313, #12465, #9361 ) ) ;
#1705 = CARTESIAN_POINT ( 'NONE',  ( -17.35186893731094671, 20.17349094513186358, 101.0000000000000000 ) ) ;
#1706 = CARTESIAN_POINT ( 'NONE',  ( 0.000000000000000000, 193.4213562373095385, -50.00000000000000000 ) ) ;
#1707 = CARTESIAN_POINT ( 'NONE',  ( 40.45084971874737079, 32.98125000068279888, -29.38926261462366440 ) ) ;
#1708 = CARTESIAN_POINT ( 'NONE',  ( 40.34137639590981905, 48.72187500034139873, 29.30972558990010768 ) ) ;
#1709 = CARTESIAN_POINT ( 'NONE',  ( 9.631387414534489405E-15, 26.35937500034140157, 52.43083105670540789 ) ) ;
#1710 = CARTESIAN_POINT ( 'NONE',  ( 5.143516556418884111E-15, 272.0000000000000000, 42.00000000000000711 ) ) ;
#1711 = AXIS2_PLACEMENT_3D ( 'NONE', #16274, #4910, #12536 ) ;
#1712 = CARTESIAN_POINT ( 'NONE',  ( 49.86468353125000164, 38.92187500034139447, -6.106662507704105588E-15 ) ) ;
#1713 = DIRECTION ( 'NONE',  ( 1.000000000000000000, 0.000000000000000000, 0.000000000000000000 ) ) ;
#1714 = CARTESIAN_POINT ( 'NONE',  ( -40.34137639590981195, 44.12187500034139731, 29.30972558990012189 ) ) ;
#1715 = CARTESIAN_POINT ( 'NONE',  ( 0.000000000000000000, 267.0000000000000000, 0.000000000000000000 ) ) ;
#1716 = VERTEX_POINT ( 'NONE', #10648 ) ;
#1717 = EDGE_CURVE ( 'NONE', #15230, #9017, #14369, .T. ) ;
#1718 = CARTESIAN_POINT ( 'NONE',  ( -30.81806926056962226, 20.15937500034139518, 42.41743335407647919 ) ) ;
#1719 = ORIENTED_EDGE ( 'NONE', *, *, #3682, .F. ) ;
#1720 = DIRECTION ( 'NONE',  ( 0.000000000000000000, 0.000000000000000000, 1.000000000000000000 ) ) ;
#1721 = EDGE_LOOP ( 'NONE', ( #9897, #11430, #1349, #3595 ) ) ;
#1722 = EDGE_CURVE ( 'NONE', #13617, #14735, #2050, .T. ) ;
#1723 = DIRECTION ( 'NONE',  ( 0.000000000000000000, 1.000000000000000000, 0.000000000000000000 ) ) ;
#1724 = FACE_OUTER_BOUND ( 'NONE', #8544, .T. ) ;
#1725 = EDGE_CURVE ( 'NONE', #13481, #11385, #10478, .T. ) ;
#1726 = DIRECTION ( 'NONE',  ( 0.000000000000000000, 0.000000000000000000, -1.000000000000000000 ) ) ;
#1727 = CARTESIAN_POINT ( 'NONE',  ( -15.45084971874737256, 25.60000000000000142, -47.55282581475767500 ) ) ;
#1728 = CARTESIAN_POINT ( 'NONE',  ( 49.86468353124999453, 42.95937500034139589, -16.20201782572376459 ) ) ;
#1729 = CARTESIAN_POINT ( 'NONE',  ( -40.45084971874737789, 31.58125000068280031, -29.38926261462365730 ) ) ;
#1730 = DIRECTION ( 'NONE',  ( 0.000000000000000000, 0.000000000000000000, 1.000000000000000000 ) ) ;
#1731 = DIRECTION ( 'NONE',  ( 1.224646799147349509E-16, 0.000000000000000000, -1.000000000000000000 ) ) ;
#1732 = EDGE_CURVE ( 'NONE', #10576, #11191, #4881, .T. ) ;
#1733 = DIRECTION ( 'NONE',  ( 6.520427397917948411E-18, -0.9396926207859082059, 0.3420201433256693790 ) ) ;
#1734 = CARTESIAN_POINT ( 'NONE',  ( 30.90169943749475578, 36.48125000068279888, 42.53254041760200010 ) ) ;
#1735 = CIRCLE ( 'NONE', #12622, 4.000000000000001776 ) ;
#1736 = DIRECTION ( 'NONE',  ( 0.5000000000000039968, -0.8660254037844363761, 0.000000000000000000 ) ) ;
#1737 = FACE_OUTER_BOUND ( 'NONE', #736, .T. ) ;
#1738 =( GEOMETRIC_REPRESENTATION_CONTEXT ( 3 ) GLOBAL_UNCERTAINTY_ASSIGNED_CONTEXT ( ( #14556 ) ) GLOBAL_UNIT_ASSIGNED_CONTEXT ( ( #9391, #6750, #13366 ) ) REPRESENTATION_CONTEXT ( 'NONE', 'WORKASPACE' ) );
#1739 = ORIENTED_EDGE ( 'NONE', *, *, #16001, .F. ) ;
#1740 = EDGE_CURVE ( 'NONE', #2027, #9264, #14507, .T. ) ;
#1741 = CARTESIAN_POINT ( 'NONE',  ( 30.81806926056964002, 36.55937500034139731, 42.41743335407647209 ) ) ;
#1742 = ORIENTED_EDGE ( 'NONE', *, *, #14552, .F. ) ;
#1743 = ORIENTED_EDGE ( 'NONE', *, *, #10491, .F. ) ;
#1744 = AXIS2_PLACEMENT_3D ( 'NONE', #14955, #16212, #4844 ) ;
#1745 = FACE_OUTER_BOUND ( 'NONE', #7603, .T. ) ;
#1746 = CARTESIAN_POINT ( 'NONE',  ( 49.86468353125000164, 22.85937500034139802, -6.106662507704105588E-15 ) ) ;
#1747 = VECTOR ( 'NONE', #4128, 1000.000000000000000 ) ;
#1748 = EDGE_LOOP ( 'NONE', ( #7738, #12625, #11533, #2666 ) ) ;
#1749 = PRODUCT_DEFINITION_SHAPE ( 'NONE', 'NONE',  #6929 ) ;
#1750 = DIRECTION ( 'NONE',  ( 0.9961946980917455452, -0.08715574274765797158, 0.000000000000000000 ) ) ;
#1751 = CARTESIAN_POINT ( 'NONE',  ( 40.45084971874737079, 35.20000000000000284, -29.38926261462366440 ) ) ;
#1752 = AXIS2_PLACEMENT_3D ( 'NONE', #4139, #11862, #4052 ) ;
#1753 = CARTESIAN_POINT ( 'NONE',  ( -3.111920190527341144E-15, 27.50000000000000000, -50.00000000000000000 ) ) ;
#1754 = CARTESIAN_POINT ( 'NONE',  ( -30.81806926056963292, 25.62187500034139731, -42.41743335407646498 ) ) ;
#1755 = DIRECTION ( 'NONE',  ( -0.9961946980917455452, 0.08715574274765797158, 0.000000000000000000 ) ) ;
#1756 = CARTESIAN_POINT ( 'NONE',  ( 0.5792196722693350175, 4.999999999999996447, 99.11836509645773674 ) ) ;
#1757 = CARTESIAN_POINT ( 'NONE',  ( 0.5000000000000000000, 39.99999999999999289, 102.0000000000000142 ) ) ;
#1758 = DIRECTION ( 'NONE',  ( -0.3213938048432631867, -0.7471788047720969717, 0.5817472440052561256 ) ) ;
#1759 = CARTESIAN_POINT ( 'NONE',  ( -1.671572875253810153, 246.1715728752537871, -50.00000000000000000 ) ) ;
#1760 = CARTESIAN_POINT ( 'NONE',  ( -3.219174618344376363E-15, 33.50000000000000711, -52.57311121191334990 ) ) ;
#1761 = CARTESIAN_POINT ( 'NONE',  ( 49.86468353124999453, 34.95937500034138878, -16.20201782572376459 ) ) ;
#1762 = CIRCLE ( 'NONE', #5243, 17.50000000000000000 ) ;
#1763 = AXIS2_PLACEMENT_3D ( 'NONE', #3834, #2583, #12728 ) ;
#1765 = EDGE_CURVE ( 'NONE', #5661, #2974, #3228, .T. ) ;
#1764 = AXIS2_PLACEMENT_3D ( 'NONE', #2525, #15236, #15157 ) ;
#1766 = CARTESIAN_POINT ( 'NONE',  ( 13.08647130699016614, 33.61029532559867050, 101.3333374614808662 ) ) ;
#1767 = VERTEX_POINT ( 'NONE', #8620 ) ;
#1768 = CARTESIAN_POINT ( 'NONE',  ( -40.34137639590981905, 29.65937500034139518, -29.30972558990011478 ) ) ;
#1769 = VERTEX_POINT ( 'NONE', #13455 ) ;
#1770 = CARTESIAN_POINT ( 'NONE',  ( 0.000000000000000000, 22.50000000000000000, 101.0000000000000000 ) ) ;
#1771 = CARTESIAN_POINT ( 'NONE',  ( 40.34137639590981195, 43.05937500034139731, -29.30972558990011834 ) ) ;
#1772 = VECTOR ( 'NONE', #11819, 1000.000000000000000 ) ;
#1773 = VECTOR ( 'NONE', #10170, 1000.000000000000000 ) ;
#1774 = CARTESIAN_POINT ( 'NONE',  ( 23.90010208165380590, 283.0244618719131040, 9.450051040827188942 ) ) ;
#1775 = VECTOR ( 'NONE', #15211, 1000.000000000000000 ) ;
#1776 = CARTESIAN_POINT ( 'NONE',  ( -28.69101924422432148, 282.0322304394514390, 11.84550962211183567 ) ) ;
#1777 = CARTESIAN_POINT ( 'NONE',  ( 30.81806926056964002, 36.62187500034139731, 42.41743335407647209 ) ) ;
#1778 = CARTESIAN_POINT ( 'NONE',  ( -30.81806926056962226, 38.15937500034139163, 42.41743335407647209 ) ) ;
#1779 = DIRECTION ( 'NONE',  ( 0.9945218953682730678, 0.1045284632676572456, 0.000000000000000000 ) ) ;
#1780 = CARTESIAN_POINT ( 'NONE',  ( 50.00000000000000711, 38.89999999999999858, 16.24598481164530739 ) ) ;
#1781 = EDGE_CURVE ( 'NONE', #842, #15320, #11663, .T. ) ;
#1782 = CARTESIAN_POINT ( 'NONE',  ( -49.99999999999999289, 23.88125000068279746, 16.24598481164533226 ) ) ;
#1783 = CARTESIAN_POINT ( 'NONE',  ( -40.34137639590981905, 41.72187500034139873, -29.30972558990011478 ) ) ;
#1784 = CARTESIAN_POINT ( 'NONE',  ( 40.34137639590981905, 24.72187500034139873, 29.30972558990010768 ) ) ;
#1785 = AXIS2_PLACEMENT_3D ( 'NONE', #10647, #9394, #14203 ) ;
#1786 = VECTOR ( 'NONE', #13203, 999.9999999999998863 ) ;
#1787 = CARTESIAN_POINT ( 'NONE',  ( 30.81806926056962936, 49.15937500034139163, -42.41743335407646498 ) ) ;
#1788 = VERTEX_POINT ( 'NONE', #12128 ) ;
#1789 = CARTESIAN_POINT ( 'NONE',  ( 50.00000000000000000, 28.78125000068279959, -6.123233995736766085E-15 ) ) ;
#1790 = ORIENTED_EDGE ( 'NONE', *, *, #2785, .T. ) ;
#1791 = LINE ( 'NONE', #13102, #1747 ) ;
#1792 = CARTESIAN_POINT ( 'NONE',  ( 30.90169943749475223, 32.48125000068280599, 42.53254041760199300 ) ) ;
#1793 = CARTESIAN_POINT ( 'NONE',  ( -15.40903463028480580, 42.32187500034139305, 47.42413220539094709 ) ) ;
#1794 = CARTESIAN_POINT ( 'NONE',  ( -40.34137639590981195, 24.05937500034139731, 29.30972558990012189 ) ) ;
#1795 = DIRECTION ( 'NONE',  ( -0.7431448254773954654, 0.6691306063588569053, 0.000000000000000000 ) ) ;
#1796 =( BOUNDED_CURVE ( )  B_SPLINE_CURVE ( 2, ( #14890, #4862, #13730, #11174, #7424, #9759, #2343, #8571, #762, #8418, #16229, #10915, #13642 ),
 .UNSPECIFIED., .F., .F. ) 
 B_SPLINE_CURVE_WITH_KNOTS ( ( 3, 2, 2, 2, 2, 2, 3 ),
 ( 0.01666666666666666990, 0.02000000000000000042, 0.02666666666666666838, 0.03333333333333333287, 0.04000000000000000083, 0.04666666666666667573, 0.05000000000000000278 ),
 .UNSPECIFIED. ) 
 CURVE ( )  GEOMETRIC_REPRESENTATION_ITEM ( )  RATIONAL_B_SPLINE_CURVE ( ( 0.9755282581475768211, 0.9755282581475768211, 1.000000000000000000, 0.9510565162951535312, 1.000000000000000000, 0.9510565162951535312, 1.000000000000000000, 0.9510565162951535312, 1.000000000000000000, 0.9510565162951535312, 1.000000000000000000, 0.9755282581475768211, 0.9755282581475768211 ) ) 
 REPRESENTATION_ITEM ( '' )  );
#1797 = CARTESIAN_POINT ( 'NONE',  ( -49.86468353124999453, 39.82187500034140015, -16.20201782572375393 ) ) ;
#1798 = EDGE_CURVE ( 'NONE', #13034, #9095, #2062, .T. ) ;
#1799 =( LENGTH_UNIT ( ) NAMED_UNIT ( * ) SI_UNIT ( .MILLI., .METRE. ) );
#1800 = CARTESIAN_POINT ( 'NONE',  ( -15.40903463028481646, 45.52187500034139589, -47.42413220539093999 ) ) ;
#1801 = CARTESIAN_POINT ( 'NONE',  ( -40.45084971874737789, 45.58125000068280031, -29.38926261462365730 ) ) ;
#1802 = ORIENTED_EDGE ( 'NONE', *, *, #7646, .F. ) ;
#1803 = CARTESIAN_POINT ( 'NONE',  ( -30.81806926056962226, 44.22187500034139163, 42.41743335407647919 ) ) ;
#1804 = ORIENTED_EDGE ( 'NONE', *, *, #1, .F. ) ;
#1805 = ORIENTED_EDGE ( 'NONE', *, *, #3028, .T. ) ;
#1806 = EDGE_CURVE ( 'NONE', #7158, #15132, #8259, .T. ) ;
#1807 = CARTESIAN_POINT ( 'NONE',  ( -5.823736356558309156E-14, 44.28125000068280315, 50.00000000000000000 ) ) ;
#1808 = CARTESIAN_POINT ( 'NONE',  ( 49.99999999999999289, 38.88125000068279036, -16.24598481164532160 ) ) ;
#1809 = CARTESIAN_POINT ( 'NONE',  ( -5.000000000000000000, 120.2608755106155201, 31.08930263536160155 ) ) ;
#1810 = CARTESIAN_POINT ( 'NONE',  ( -50.00000000000000000, 28.00000000000000000, 0.000000000000000000 ) ) ;
#1811 = CARTESIAN_POINT ( 'NONE',  ( 30.81806926056962936, 41.15937500034139873, -42.41743335407647209 ) ) ;
#1812 = DIRECTION ( 'NONE',  ( -0.5000000000000041078, 0.000000000000000000, -0.8660254037844363761 ) ) ;
#1813 = CARTESIAN_POINT ( 'NONE',  ( -5.000000000000000000, 58.69043703438383375, 45.69588935894790183 ) ) ;
#1814 = CARTESIAN_POINT ( 'NONE',  ( -15.45084971874737256, 45.60000000000000142, -47.55282581475767500 ) ) ;
#1815 = CARTESIAN_POINT ( 'NONE',  ( 0.000000000000000000, 242.0000000000000284, 0.000000000000000000 ) ) ;
#1816 = CARTESIAN_POINT ( 'NONE',  ( -40.45084971874737079, 33.98125000068279888, 29.38926261462367151 ) ) ;
#1817 = CARTESIAN_POINT ( 'NONE',  ( 1.293669679204937499E-13, 37.50000000000000711, -50.00000000000000000 ) ) ;
#1818 = EDGE_CURVE ( 'NONE', #7740, #9508, #1453, .T. ) ;
#1819 = VERTEX_POINT ( 'NONE', #7313 ) ;
#1820 = CARTESIAN_POINT ( 'NONE',  ( -40.34137639590981195, 30.05937500034139731, 29.30972558990012189 ) ) ;
#1821 = ORIENTED_EDGE ( 'NONE', *, *, #7453, .T. ) ;
#1822 = ORIENTED_EDGE ( 'NONE', *, *, #13766, .T. ) ;
#1823 = CARTESIAN_POINT ( 'NONE',  ( 7.919222016226854954, 42.55125428154684641, 49.99999999999998579 ) ) ;
#1824 = CARTESIAN_POINT ( 'NONE',  ( -37.77664397204053159, 25.00000000000000355, -13.15010152849376190 ) ) ;
#1825 = CARTESIAN_POINT ( 'NONE',  ( -2.500000000000000000, 242.0000000000000284, -40.00000000000000000 ) ) ;
#1826 = ORIENTED_EDGE ( 'NONE', *, *, #1221, .T. ) ;
#1827 = CARTESIAN_POINT ( 'NONE',  ( -10.09851121871618140, 9.451242543235633065, 102.0000000000000142 ) ) ;
#1828 = CARTESIAN_POINT ( 'NONE',  ( 15.45084971874737789, 34.60000000000000853, 47.55282581475767500 ) ) ;
#1829 = FACE_OUTER_BOUND ( 'NONE', #13462, .T. ) ;
#1830 = CARTESIAN_POINT ( 'NONE',  ( -40.34137639590981195, 30.12187500034139731, 29.30972558990012189 ) ) ;
#1831 = ADVANCED_FACE ( 'NONE', ( #734 ), #8442, .T. ) ;
#1832 = CARTESIAN_POINT ( 'NONE',  ( -15.45084971874737256, 37.38125000068279746, -47.55282581475767500 ) ) ;
#1833 = CARTESIAN_POINT ( 'NONE',  ( 50.00000000000000000, 47.00000000000000000, -6.123233995736766085E-15 ) ) ;
#1834 = CARTESIAN_POINT ( 'NONE',  ( -46.96694430692108568, 19.99999999999999645, 16.75173377947249165 ) ) ;
#1835 = CARTESIAN_POINT ( 'NONE',  ( 15.40903463028481113, 23.32187500034139660, -47.42413220539094709 ) ) ;
#1836 = CARTESIAN_POINT ( 'NONE',  ( 3.147895402236133400, 5.285449336779636909, 101.0000000000000000 ) ) ;
#1837 = CARTESIAN_POINT ( 'NONE',  ( -30.90169943749474868, 35.69999999999999574, -42.53254041760200721 ) ) ;
#1838 = CARTESIAN_POINT ( 'NONE',  ( 30.81806926056964002, 26.55937500034139376, 42.41743335407647209 ) ) ;
#1839 = CYLINDRICAL_SURFACE ( 'NONE', #13610, 50.00000000000000000 ) ;
#1840 = VERTEX_POINT ( 'NONE', #7795 ) ;
#1841 = EDGE_CURVE ( 'NONE', #7924, #286, #1384, .T. ) ;
#1842 = CARTESIAN_POINT ( 'NONE',  ( 49.86468353124999453, 30.95937500034139944, -16.20201782572376104 ) ) ;
#1843 = ORIENTED_EDGE ( 'NONE', *, *, #16366, .F. ) ;
#1844 = DIRECTION ( 'NONE',  ( -0.000000000000000000, -1.000000000000000000, -0.000000000000000000 ) ) ;
#1845 = CARTESIAN_POINT ( 'NONE',  ( -40.34137639590981195, 40.05937500034140442, 29.30972558990012189 ) ) ;
#1846 = AXIS2_PLACEMENT_3D ( 'NONE', #12793, #145, #15039 ) ;
#1847 = CARTESIAN_POINT ( 'NONE',  ( -49.86468353124999453, 20.02187500034139589, 16.20201782572377525 ) ) ;
#1848 = CARTESIAN_POINT ( 'NONE',  ( -7.500000000000000000, 40.00000000000000711, -39.29058411375427795 ) ) ;
#1849 = CARTESIAN_POINT ( 'NONE',  ( 15.40903463028482356, 32.52187500034139589, 47.42413220539093999 ) ) ;
#1850 = CARTESIAN_POINT ( 'NONE',  ( -3.210462471511496205E-15, 35.35937500034140157, -52.43083105670540789 ) ) ;
#1851 = CARTESIAN_POINT ( 'NONE',  ( 7.500000000000005329, 25.00000000000000355, -24.29058411375428506 ) ) ;
#1852 = CARTESIAN_POINT ( 'NONE',  ( 49.86468353124999453, 29.02187500034139234, -16.20201782572376459 ) ) ;
#1853 = CARTESIAN_POINT ( 'NONE',  ( 9.657523855033129090E-15, 40.50000000000000711, 52.57311121191334990 ) ) ;
#1854 = CARTESIAN_POINT ( 'NONE',  ( 30.90169943749475578, 20.48125000068279178, 42.53254041760200010 ) ) ;
#1855 = CARTESIAN_POINT ( 'NONE',  ( 40.34137639590981195, 45.12187500034139731, -29.30972558990011834 ) ) ;
#1856 = CARTESIAN_POINT ( 'NONE',  ( 40.45084971874737079, 49.20000000000000284, -29.38926261462366440 ) ) ;
#1857 = EDGE_CURVE ( 'NONE', #3799, #8474, #14802, .T. ) ;
#1858 = ORIENTED_EDGE ( 'NONE', *, *, #1565, .T. ) ;
#1859 = ADVANCED_FACE ( 'NONE', ( #12864 ), #16446, .F. ) ;
#1860 = CARTESIAN_POINT ( 'NONE',  ( -40.34137639590981195, 46.05937500034139731, 29.30972558990012189 ) ) ;
#1861 = EDGE_LOOP ( 'NONE', ( #9094, #13992, #14105, #15765 ) ) ;
#1862 = CARTESIAN_POINT ( 'NONE',  ( 50.00000000000000711, 28.68125000068279462, 16.24598481164530739 ) ) ;
#1863 = VERTEX_POINT ( 'NONE', #6315 ) ;
#1864 = FACE_OUTER_BOUND ( 'NONE', #13111, .T. ) ;
#1865 = CARTESIAN_POINT ( 'NONE',  ( 0.000000000000000000, 217.0000000000000284, 0.000000000000000000 ) ) ;
#1866 = CARTESIAN_POINT ( 'NONE',  ( -49.86468353125000164, 41.92187500034139447, 0.000000000000000000 ) ) ;
#1867 = CARTESIAN_POINT ( 'NONE',  ( -30.81806926056962226, 28.15937500034139518, 42.41743335407647919 ) ) ;
#1868 = CARTESIAN_POINT ( 'NONE',  ( -3.505380114644271572, 97.73782665365224887, -8.566253778398380092 ) ) ;
#1869 = ITEM_DEFINED_TRANSFORMATION ( 'NONE', 'NONE', #12918,  #15812 ) ;
#1870 = CARTESIAN_POINT ( 'NONE',  ( 40.45084971874737789, 34.80000000000000426, 29.38926261462365375 ) ) ;
#1871 = EDGE_CURVE ( 'NONE', #1062, #5162, #15872, .T. ) ;
#1872 = CARTESIAN_POINT ( 'NONE',  ( -15.40903463028481646, 43.52187500034139589, -47.42413220539093999 ) ) ;
#1873 = EDGE_CURVE ( 'NONE', #2880, #10320, #13746, .T. ) ;
#1874 = CARTESIAN_POINT ( 'NONE',  ( 0.000000000000000000, 52.00000000000000711, 0.000000000000000000 ) ) ;
#1875 = ORIENTED_EDGE ( 'NONE', *, *, #125, .F. ) ;
#1876 = CARTESIAN_POINT ( 'NONE',  ( 49.86468353125001585, 40.82187500034140726, 16.20201782572375038 ) ) ;
#1877 = PRODUCT ( 'container base & motor', 'container base & motor', '', ( #788 ) ) ;
#1878 = ORIENTED_EDGE ( 'NONE', *, *, #3264, .F. ) ;
#1879 = VERTEX_POINT ( 'NONE', #11455 ) ;
#1880 = EDGE_CURVE ( 'NONE', #3644, #8369, #7005, .T. ) ;
#1881 = DIRECTION ( 'NONE',  ( -0.000000000000000000, 1.000000000000000000, -0.000000000000000000 ) ) ;
#1882 = DIRECTION ( 'NONE',  ( -0.000000000000000000, -1.000000000000000000, -0.000000000000000000 ) ) ;
#1883 =( BOUNDED_CURVE ( )  B_SPLINE_CURVE ( 3, ( #11422, #10668, #1759, #14143 ),
 .UNSPECIFIED., .F., .F. ) 
 B_SPLINE_CURVE_WITH_KNOTS ( ( 4, 4 ),
 ( 3.141592653589793116, 4.712388980384689674 ),
 .UNSPECIFIED. ) 
 CURVE ( )  GEOMETRIC_REPRESENTATION_ITEM ( )  RATIONAL_B_SPLINE_CURVE ( ( 1.000000000000000000, 0.8047378541243649375, 0.8047378541243649375, 1.000000000000000000 ) ) 
 REPRESENTATION_ITEM ( '' )  );
#1884 = LINE ( 'NONE', #10638, #2647 ) ;
#1885 = CARTESIAN_POINT ( 'NONE',  ( 30.90169943749475578, 20.69999999999999574, 42.53254041760200010 ) ) ;
#1886 = CARTESIAN_POINT ( 'NONE',  ( 40.34137639590981905, 44.65937500034139163, 29.30972558990010768 ) ) ;
#1887 = DIRECTION ( 'NONE',  ( 0.8660254037844434816, -0.000000000000000000, 0.4999999999999916733 ) ) ;
#1888 = CARTESIAN_POINT ( 'NONE',  ( 48.69930661242913317, 95.73172307475270770, 7.581784256837345914 ) ) ;
#1889 = CARTESIAN_POINT ( 'NONE',  ( 0.000000000000000000, 193.4213562373095385, 0.000000000000000000 ) ) ;
#1890 = DIRECTION ( 'NONE',  ( 0.9961946980917455452, -0.08715574274765795770, 0.000000000000000000 ) ) ;
#1891 = CARTESIAN_POINT ( 'NONE',  ( 0.000000000000000000, 252.1309828287255357, 79.49773270518484480 ) ) ;
#1892 = CARTESIAN_POINT ( 'NONE',  ( 49.99999999999999289, 37.10000000000000142, -16.24598481164532160 ) ) ;
#1893 = ORIENTED_EDGE ( 'NONE', *, *, #1112, .F. ) ;
#1894 = CARTESIAN_POINT ( 'NONE',  ( 49.86468353125001585, 28.75937500034139305, 16.20201782572375038 ) ) ;
#1895 = ORIENTED_EDGE ( 'NONE', *, *, #7141, .F. ) ;
#1896 = ORIENTED_EDGE ( 'NONE', *, *, #13712, .F. ) ;
#1897 = ORIENTED_EDGE ( 'NONE', *, *, #13064, .F. ) ;
#1898 = CARTESIAN_POINT ( 'NONE',  ( 50.00000000000000000, 42.78125000068280315, -6.123233995736766085E-15 ) ) ;
#1899 = FACE_OUTER_BOUND ( 'NONE', #3217, .T. ) ;
#1900 = CARTESIAN_POINT ( 'NONE',  ( -15.40903463028481646, 25.45937500034139589, -47.42413220539093999 ) ) ;
#1901 = ORIENTED_EDGE ( 'NONE', *, *, #5685, .F. ) ;
#1902 = CARTESIAN_POINT ( 'NONE',  ( -15.45084971874737256, 27.38125000068280102, -47.55282581475767500 ) ) ;
#1903 = CARTESIAN_POINT ( 'NONE',  ( -3.918041248536338728, 6.471932344328960696, 102.0000000000000142 ) ) ;
#1904 = CARTESIAN_POINT ( 'NONE',  ( 15.45084971874736723, 23.40000000000000213, -47.55282581475768211 ) ) ;
#1905 = CARTESIAN_POINT ( 'NONE',  ( 0.000000000000000000, 193.4213562373095385, 0.000000000000000000 ) ) ;
#1906 = CARTESIAN_POINT ( 'NONE',  ( -49.86468353124999453, 29.82187500034139660, -16.20201782572375393 ) ) ;
#1907 = CARTESIAN_POINT ( 'NONE',  ( -15.45084971874736368, 32.39999999999999858, 47.55282581475768211 ) ) ;
#1908 = CARTESIAN_POINT ( 'NONE',  ( 8.850089126414076190, 7.391638089289761737, 98.30041665922365723 ) ) ;
#1909 = CARTESIAN_POINT ( 'NONE',  ( -45.47188453826096577, 20.00000000000001066, 20.46517872429623353 ) ) ;
#1910 = CARTESIAN_POINT ( 'NONE',  ( 9.631387414534489405E-15, 22.42187500034139802, 52.43083105670540789 ) ) ;
#1911 = CARTESIAN_POINT ( 'NONE',  ( 0.000000000000000000, 242.0000000000000284, 0.000000000000000000 ) ) ;
#1912 = CARTESIAN_POINT ( 'NONE',  ( -50.00000000000000000, 32.00000000000000000, 0.000000000000000000 ) ) ;
#1913 = CARTESIAN_POINT ( 'NONE',  ( 15.40903463028481113, 27.25937500034139660, -47.42413220539094709 ) ) ;
#1914 = CARTESIAN_POINT ( 'NONE',  ( -8.660254037844415720, 45.00000000000001421, -4.999999999999952927 ) ) ;
#1915 = ORIENTED_EDGE ( 'NONE', *, *, #6442, .F. ) ;
#1916 = ADVANCED_FACE ( 'NONE', ( #9964 ), #7549, .T. ) ;
#1917 = VECTOR ( 'NONE', #11886, 1000.000000000000114 ) ;
#1918 = UNCERTAINTY_MEASURE_WITH_UNIT (LENGTH_MEASURE( 1.000000000000000082E-05 ), #12798, 'distance_accuracy_value', 'NONE');
#1919 = CARTESIAN_POINT ( 'NONE',  ( 30.81806926056962936, 29.15937500034139518, -42.41743335407646498 ) ) ;
#1920 = ORIENTED_EDGE ( 'NONE', *, *, #7912, .T. ) ;
#1921 = CARTESIAN_POINT ( 'NONE',  ( 14.90544456622775904, 13.31698729810792692, 101.0000000000000000 ) ) ;
#1922 = CARTESIAN_POINT ( 'NONE',  ( 40.34137639590981905, 44.65937500034139163, 29.30972558990010768 ) ) ;
#1923 = CARTESIAN_POINT ( 'NONE',  ( 21.32168401022777360, 284.4942466288916307, 8.160842005118437825 ) ) ;
#1924 = EDGE_CURVE ( 'NONE', #13942, #2064, #13776, .T. ) ;
#1925 = ADVANCED_FACE ( 'NONE', ( #2470 ), #2388, .F. ) ;
#1926 = CARTESIAN_POINT ( 'NONE',  ( 2.281160512027670796E-15, 45.00000000000001421, -3.951085907051776750E-15 ) ) ;
#1927 = CARTESIAN_POINT ( 'NONE',  ( -30.81806926056963292, 31.62187500034139731, -42.41743335407647209 ) ) ;
#1928 = CARTESIAN_POINT ( 'NONE',  ( 49.86468353125000164, 36.85937500034139447, -6.106662507704105588E-15 ) ) ;
#1929 = DIRECTION ( 'NONE',  ( 0.4067366430758010964, -0.9135454576426004225, 0.000000000000000000 ) ) ;
#1930 = CARTESIAN_POINT ( 'NONE',  ( 9.631387414534489405E-15, 28.42187500034139092, 52.43083105670540789 ) ) ;
#1931 = DIRECTION ( 'NONE',  ( 0.000000000000000000, 1.000000000000000000, 0.000000000000000000 ) ) ;
#1932 = VECTOR ( 'NONE', #15469, 999.9999999999998863 ) ;
#1933 = EDGE_CURVE ( 'NONE', #8272, #81, #7384, .T. ) ;
#1934 = CARTESIAN_POINT ( 'NONE',  ( -49.86468353124999453, 43.75937500034140015, -16.20201782572375393 ) ) ;
#1935 = CARTESIAN_POINT ( 'NONE',  ( 30.81806926056964002, 44.62187500034140442, 42.41743335407647209 ) ) ;
#1936 = CARTESIAN_POINT ( 'NONE',  ( -49.86468353124999453, 24.02187500034139589, 16.20201782572377525 ) ) ;
#1937 = ORIENTED_EDGE ( 'NONE', *, *, #14545, .T. ) ;
#1938 = ADVANCED_FACE ( 'NONE', ( #16357, #4997 ), #2715, .F. ) ;
#1939 = FACE_OUTER_BOUND ( 'NONE', #2477, .T. ) ;
#1940 = ORIENTED_EDGE ( 'NONE', *, *, #7735, .F. ) ;
#1941 = EDGE_LOOP ( 'NONE', ( #13863, #12708 ) ) ;
#1942 = CARTESIAN_POINT ( 'NONE',  ( -50.00000000000000000, 27.78125000068279959, 0.000000000000000000 ) ) ;
#1943 = CIRCLE ( 'NONE', #7794, 45.00000000000000000 ) ;
#1944 = ORIENTED_EDGE ( 'NONE', *, *, #5416, .F. ) ;
#1945 = CARTESIAN_POINT ( 'NONE',  ( 3.918041248536554555, 6.471932344329013098, 102.0000000000000142 ) ) ;
#1946 = CARTESIAN_POINT ( 'NONE',  ( -40.34137639590981195, 38.12187500034139731, 29.30972558990012189 ) ) ;
#1947 = CARTESIAN_POINT ( 'NONE',  ( 30.81806926056964002, 46.62187500034140442, 42.41743335407647209 ) ) ;
#1948 = CARTESIAN_POINT ( 'NONE',  ( 0.000000000000000000, 22.50000000000000000, 102.0000000000000142 ) ) ;
#1949 = CARTESIAN_POINT ( 'NONE',  ( 49.99999999999999289, 37.10000000000000142, -16.24598481164532160 ) ) ;
#1950 = AXIS2_PLACEMENT_3D ( 'NONE', #12374, #11049, #974 ) ;
#1951 = CARTESIAN_POINT ( 'NONE',  ( 30.81806926056964002, 40.62187500034139731, 42.41743335407647209 ) ) ;
#1952 = CARTESIAN_POINT ( 'NONE',  ( -49.99999999999999289, 45.88125000068279746, 16.24598481164533226 ) ) ;
#1953 = ORIENTED_EDGE ( 'NONE', *, *, #1542, .T. ) ;
#1954 = CARTESIAN_POINT ( 'NONE',  ( -49.86468353124999453, 39.82187500034140015, -16.20201782572375393 ) ) ;
#1955 = ORIENTED_EDGE ( 'NONE', *, *, #14733, .T. ) ;
#1956 = ORIENTED_EDGE ( 'NONE', *, *, #8034, .T. ) ;
#1957 = EDGE_LOOP ( 'NONE', ( #12978, #13764, #4666, #14845 ) ) ;
#1958 = CARTESIAN_POINT ( 'NONE',  ( 2.600676159226421000E-13, 23.50000000000000000, -49.99999999999999289 ) ) ;
#1959 = DIRECTION ( 'NONE',  ( 0.000000000000000000, 0.000000000000000000, -1.000000000000000000 ) ) ;
#1960 = CIRCLE ( 'NONE', #12861, 42.00000000000000711 ) ;
#1961 = CARTESIAN_POINT ( 'NONE',  ( 0.000000000000000000, 55.00000000000000711, 62.25100647794772613 ) ) ;
#1962 = DIRECTION ( 'NONE',  ( -0.000000000000000000, 1.000000000000000000, -0.000000000000000000 ) ) ;
#1963 = CARTESIAN_POINT ( 'NONE',  ( 49.86468353125000164, 40.85937500034139447, -6.106662507704105588E-15 ) ) ;
#1964 = DIRECTION ( 'NONE',  ( 5.069245582283711292E-17, 1.000000000000000000, -8.780190904559502465E-17 ) ) ;
#1965 = CARTESIAN_POINT ( 'NONE',  ( 0.000000000000000000, 261.9999999999999432, 0.000000000000000000 ) ) ;
#1966 = DIRECTION ( 'NONE',  ( 0.000000000000000000, 1.000000000000000000, 0.000000000000000000 ) ) ;
#1967 =( LENGTH_UNIT ( ) NAMED_UNIT ( * ) SI_UNIT ( .MILLI., .METRE. ) );
#1968 = CARTESIAN_POINT ( 'NONE',  ( 2.499999999999999556, 242.0000000000000284, -49.17157287525379417 ) ) ;
#1969 = LINE ( 'NONE', #4568, #8682 ) ;
#1970 = CARTESIAN_POINT ( 'NONE',  ( 50.00000000000000711, 42.68125000068280173, 16.24598481164530739 ) ) ;
#1971 = EDGE_CURVE ( 'NONE', #13357, #6818, #8791, .T. ) ;
#1972 = CARTESIAN_POINT ( 'NONE',  ( 0.000000000000000000, 25.00000000000000355, 0.000000000000000000 ) ) ;
#1973 = ORIENTED_EDGE ( 'NONE', *, *, #10109, .F. ) ;
#1974 = COLOUR_RGB ( '', 0.08235294, 0.09019608, 0.10196078) ;
#1975 = CARTESIAN_POINT ( 'NONE',  ( -30.81806926056963292, 29.55937500034139376, -42.41743335407647209 ) ) ;
#1976 = EDGE_LOOP ( 'NONE', ( #5329, #7799, #7517, #2611 ) ) ;
#1977 = VERTEX_POINT ( 'NONE', #11381 ) ;
#1978 = ORIENTED_EDGE ( 'NONE', *, *, #9479, .T. ) ;
#1979 =( BOUNDED_CURVE ( )  B_SPLINE_CURVE ( 2, ( #12632, #2652, #1568, #10468, #3987, #15526, #12877, #3908, #6661, #6328, #9059, #2727, #2482 ),
 .UNSPECIFIED., .F., .T. ) 
 B_SPLINE_CURVE_WITH_KNOTS ( ( 3, 2, 2, 2, 2, 2, 3 ),
 ( 0.6833333333333333481, 0.6866666666666666474, 0.6933333333333333570, 0.6999999999999999556, 0.7066666666666666652, 0.7133333333333333748, 0.7166666666666666741 ),
 .UNSPECIFIED. ) 
 CURVE ( )  GEOMETRIC_REPRESENTATION_ITEM ( )  RATIONAL_B_SPLINE_CURVE ( ( 0.9755282581475768211, 0.9755282581475768211, 1.000000000000000000, 0.9510565162951535312, 1.000000000000000000, 0.9510565162951535312, 1.000000000000000000, 0.9510565162951535312, 1.000000000000000000, 0.9510565162951535312, 1.000000000000000000, 0.9755282581475768211, 0.9755282581475768211 ) ) 
 REPRESENTATION_ITEM ( '' )  );
#1980 = CARTESIAN_POINT ( 'NONE',  ( 40.45084971874737789, 44.58125000068280031, 29.38926261462365375 ) ) ;
#1981 = DIRECTION ( 'NONE',  ( 0.000000000000000000, 0.000000000000000000, 1.000000000000000000 ) ) ;
#1982 = PRESENTATION_STYLE_ASSIGNMENT (( #14868 ) ) ;
#1983 = EDGE_LOOP ( 'NONE', ( #585, #8284, #2592, #12178 ) ) ;
#1984 = CARTESIAN_POINT ( 'NONE',  ( 0.000000000000000000, 20.00000000000000355, 0.000000000000000000 ) ) ;
#1985 = DIRECTION ( 'NONE',  ( -1.000000000000000000, 0.000000000000000000, -1.734723475976807094E-17 ) ) ;
#1986 = CARTESIAN_POINT ( 'NONE',  ( -17.50000000000000000, 22.50000000000000000, 102.0000000000000142 ) ) ;
#1987 = CARTESIAN_POINT ( 'NONE',  ( 7.919222016226693306, 34.55125428154684641, 50.00000000000003553 ) ) ;
#1988 = FACE_OUTER_BOUND ( 'NONE', #11505, .T. ) ;
#1989 = CARTESIAN_POINT ( 'NONE',  ( 0.1743114854953164983, 100.0076106038165165, 5.000000000000000000 ) ) ;
#1990 = VECTOR ( 'NONE', #11855, 1000.000000000000000 ) ;
#1991 = DIRECTION ( 'NONE',  ( 0.000000000000000000, 0.000000000000000000, -1.000000000000000000 ) ) ;
#1992 = CARTESIAN_POINT ( 'NONE',  ( 37.77664397204061686, 40.00000000000000711, 13.15010152849349900 ) ) ;
#1993 = CARTESIAN_POINT ( 'NONE',  ( 0.000000000000000000, 25.00000000000000000, -47.00000000000000000 ) ) ;
#1994 = B_SPLINE_CURVE_WITH_KNOTS ( 'NONE', 3,
 ( #13386, #752, #5839, #10905 ),
 .UNSPECIFIED., .F., .F.,
 ( 4, 4 ),
 ( 0.000000000000000000, 0.01241723871866209916 ),
 .UNSPECIFIED. ) ;
#1995 = CARTESIAN_POINT ( 'NONE',  ( -3.210462471511496205E-15, 21.42187500034139802, -52.43083105670540789 ) ) ;
#1996 = DIRECTION ( 'NONE',  ( -6.938893903907231459E-18, 1.000000000000000000, 5.551115123125782702E-17 ) ) ;
#1997 = CARTESIAN_POINT ( 'NONE',  ( -50.00000000000000000, 28.00000000000000000, 0.000000000000000000 ) ) ;
#1998 = CARTESIAN_POINT ( 'NONE',  ( 40.34137639590981195, 23.05937500034139731, -29.30972558990011834 ) ) ;
#1999 = CARTESIAN_POINT ( 'NONE',  ( 0.000000000000000000, 252.0000000000000000, 82.49773270518484480 ) ) ;
#2000 = EDGE_LOOP ( 'NONE', ( #3155, #11326, #2184, #1973 ) ) ;
#2001 = AXIS2_PLACEMENT_3D ( 'NONE', #6202, #15242, #4030 ) ;
#2002 = VECTOR ( 'NONE', #16137, 1000.000000000000000 ) ;
#2003 = CARTESIAN_POINT ( 'NONE',  ( 15.45084971874736723, 45.40000000000000568, -47.55282581475768211 ) ) ;
#2004 = ORIENTED_EDGE ( 'NONE', *, *, #16114, .T. ) ;
#2005 = MECHANICAL_DESIGN_GEOMETRIC_PRESENTATION_REPRESENTATION (  '', ( #13426 ), #15828 ) ;
#2006 = FACE_OUTER_BOUND ( 'NONE', #5801, .T. ) ;
#2007 = CARTESIAN_POINT ( 'NONE',  ( -49.86468353124999453, 33.75937500034140015, -16.20201782572375393 ) ) ;
#2008 = EDGE_CURVE ( 'NONE', #5355, #10616, #15181, .T. ) ;
#2009 = ADVANCED_FACE ( 'NONE', ( #15434 ), #3605, .F. ) ;
#2010 = DIRECTION ( 'NONE',  ( 0.000000000000000000, 0.000000000000000000, 1.000000000000000000 ) ) ;
#2011 = CARTESIAN_POINT ( 'NONE',  ( 25.00000000000000000, 287.0000000000000568, 2.500000000000001776 ) ) ;
#2012 = CARTESIAN_POINT ( 'NONE',  ( -25.00000000000001066, 287.0000000000000000, 7.500000000000002665 ) ) ;
#2013 = CARTESIAN_POINT ( 'NONE',  ( 49.86468353125000164, 28.92187500034139802, -6.106662507704105588E-15 ) ) ;
#2014 = CARTESIAN_POINT ( 'NONE',  ( 49.86468353124999453, 28.95937500034139589, -16.20201782572376104 ) ) ;
#2015 = VECTOR ( 'NONE', #7830, 1000.000000000000000 ) ;
#2016 = CIRCLE ( 'NONE', #8120, 79.49773270518484480 ) ;
#2017 = FACE_OUTER_BOUND ( 'NONE', #8126, .T. ) ;
#2018 = CARTESIAN_POINT ( 'NONE',  ( -15.40903463028480580, 30.32187500034140015, 47.42413220539094709 ) ) ;
#2019 = VECTOR ( 'NONE', #16042, 1000.000000000000000 ) ;
#2020 = CARTESIAN_POINT ( 'NONE',  ( 9.041411772857449839E-15, 53.82568851450475478, -65.15972704814865324 ) ) ;
#2021 = CARTESIAN_POINT ( 'NONE',  ( -15.40903463028480580, 48.25937500034140015, 47.42413220539094709 ) ) ;
#2022 = CARTESIAN_POINT ( 'NONE',  ( -30.81806926056963292, 39.62187500034138310, -42.41743335407647209 ) ) ;
#2023 = CARTESIAN_POINT ( 'NONE',  ( 15.40903463028482356, 20.52187500034139589, 47.42413220539093999 ) ) ;
#2024 = EDGE_CURVE ( 'NONE', #10428, #13519, #881, .T. ) ;
#2025 = ORIENTED_EDGE ( 'NONE', *, *, #13441, .T. ) ;
#2026 = CARTESIAN_POINT ( 'NONE',  ( -40.34137639590981905, 41.65937500034139873, -29.30972558990011478 ) ) ;
#2027 = VERTEX_POINT ( 'NONE', #725 ) ;
#2028 = MECHANICAL_DESIGN_GEOMETRIC_PRESENTATION_REPRESENTATION (  '', ( #13447 ), #954 ) ;
#2030 = CARTESIAN_POINT ( 'NONE',  ( -49.99999999999999289, 33.88125000068280457, 16.24598481164533226 ) ) ;
#2029 = AXIS2_PLACEMENT_3D ( 'NONE', #11411, #2419, #1253 ) ;
#2031 = VERTEX_POINT ( 'NONE', #12201 ) ;
#2032 =( BOUNDED_CURVE ( )  B_SPLINE_CURVE ( 2, ( #4354, #15570, #6864, #15480, #15169, #432, #7922, #1289, #346, #10507, #10118, #1680, #14463 ),
 .UNSPECIFIED., .F., .F. ) 
 B_SPLINE_CURVE_WITH_KNOTS ( ( 3, 2, 2, 2, 2, 2, 3 ),
 ( 0.3500000000000000333, 0.3533333333333333326, 0.3599999999999999867, 0.3666666666666666408, 0.3733333333333333504, 0.3800000000000000044, 0.3833333333333333592 ),
 .UNSPECIFIED. ) 
 CURVE ( )  GEOMETRIC_REPRESENTATION_ITEM ( )  RATIONAL_B_SPLINE_CURVE ( ( 0.9755282581475768211, 0.9755282581475770431, 1.000000000000000000, 0.9510565162951535312, 1.000000000000000000, 0.9510565162951535312, 1.000000000000000000, 0.9510565162951535312, 1.000000000000000000, 0.9510565162951535312, 1.000000000000000000, 0.9755282581475765991, 0.9755282581475768211 ) ) 
 REPRESENTATION_ITEM ( '' )  );
#2033 = CARTESIAN_POINT ( 'NONE',  ( 7.919222016226758143, 40.33250428222964246, 50.00000000000000711 ) ) ;
#2034 = CARTESIAN_POINT ( 'NONE',  ( 30.81806926056962936, 43.22187500034139873, -42.41743335407646498 ) ) ;
#2035 = CARTESIAN_POINT ( 'NONE',  ( -40.34137639590981195, 20.05937500034139731, 29.30972558990012189 ) ) ;
#2036 = CARTESIAN_POINT ( 'NONE',  ( 0.000000000000000000, 20.00000000000000355, 50.00000000000000000 ) ) ;
#2037 = EDGE_CURVE ( 'NONE', #16127, #5607, #11137, .T. ) ;
#2038 = CARTESIAN_POINT ( 'NONE',  ( 15.40903463028482356, 24.52187500034139589, 47.42413220539093999 ) ) ;
#2039 = VECTOR ( 'NONE', #16120, 1000.000000000000114 ) ;
#2040 = CARTESIAN_POINT ( 'NONE',  ( 50.00000000000000000, 37.00000000000000711, -6.123233995736766085E-15 ) ) ;
#2041 = VECTOR ( 'NONE', #1043, 1000.000000000000000 ) ;
#2042 = CARTESIAN_POINT ( 'NONE',  ( -49.86468353124999453, 38.02187500034140299, 16.20201782572377525 ) ) ;
#2043 = LINE ( 'NONE', #7132, #15998 ) ;
#2044 = ORIENTED_EDGE ( 'NONE', *, *, #16095, .T. ) ;
#2045 = CARTESIAN_POINT ( 'NONE',  ( 49.86468353124999453, 39.02187500034138878, -16.20201782572376459 ) ) ;
#2046 = ADVANCED_FACE ( 'NONE', ( #9713 ), #3396, .F. ) ;
#2047 = ORIENTED_EDGE ( 'NONE', *, *, #1166, .F. ) ;
#2048 = ORIENTED_EDGE ( 'NONE', *, *, #1434, .T. ) ;
#2049 = EDGE_CURVE ( 'NONE', #12110, #4234, #733, .T. ) ;
#2050 = CIRCLE ( 'NONE', #1255, 5.000000000000000000 ) ;
#2051 = VERTEX_POINT ( 'NONE', #16020 ) ;
#2052 = DIRECTION ( 'NONE',  ( 0.000000000000000000, 1.000000000000000000, 0.000000000000000000 ) ) ;
#2053 = DIRECTION ( 'NONE',  ( 0.000000000000000000, 0.000000000000000000, -1.000000000000000000 ) ) ;
#2054 = CARTESIAN_POINT ( 'NONE',  ( -2.500000000000000000, 242.0000000000000284, 47.99999999999999289 ) ) ;
#2055 = CARTESIAN_POINT ( 'NONE',  ( 15.45084971874736723, 37.18125000068280173, -47.55282581475768211 ) ) ;
#2056 = CARTESIAN_POINT ( 'NONE',  ( 9.631387414534489405E-15, 36.35937500034140157, 52.43083105670540789 ) ) ;
#2057 = CARTESIAN_POINT ( 'NONE',  ( 15.40903463028482356, 46.45937500034139589, 47.42413220539093999 ) ) ;
#2058 = DIRECTION ( 'NONE',  ( 0.9961946980917455452, 0.08715574274765823526, -0.000000000000000000 ) ) ;
#2059 = CARTESIAN_POINT ( 'NONE',  ( -0.5000000000000000000, 244.0000000000000284, 49.99999999999999289 ) ) ;
#2060 = CARTESIAN_POINT ( 'NONE',  ( 15.83973438765496056, 27.12091057352781931, 102.0000000000000142 ) ) ;
#2061 = DIRECTION ( 'NONE',  ( 0.000000000000000000, 0.000000000000000000, 1.000000000000000000 ) ) ;
#2062 = LINE ( 'NONE', #8382, #3390 ) ;
#2063 = CARTESIAN_POINT ( 'NONE',  ( -7.571758127758879908, 38.27715053026740577, 101.0000000000000000 ) ) ;
#2064 = VERTEX_POINT ( 'NONE', #14677 ) ;
#2065 = CARTESIAN_POINT ( 'NONE',  ( 30.81806926056962936, 29.15937500034139518, -42.41743335407647209 ) ) ;
#2066 = ORIENTED_EDGE ( 'NONE', *, *, #6208, .F. ) ;
#2067 = ORIENTED_EDGE ( 'NONE', *, *, #5119, .F. ) ;
#2068 = ORIENTED_EDGE ( 'NONE', *, *, #7249, .T. ) ;
#2069 = ADVANCED_FACE ( 'NONE', ( #3305 ), #9800, .T. ) ;
#2070 = CARTESIAN_POINT ( 'NONE',  ( -15.45084971874736368, 44.18125000068280173, 47.55282581475768211 ) ) ;
#2071 = CARTESIAN_POINT ( 'NONE',  ( -5.000000000000000000, 126.6482322781408953, 36.06244584051386681 ) ) ;
#2072 =( NAMED_UNIT ( * ) SI_UNIT ( $, .STERADIAN. ) SOLID_ANGLE_UNIT ( ) );
#2073 = ORIENTED_EDGE ( 'NONE', *, *, #3686, .F. ) ;
#2074 = CARTESIAN_POINT ( 'NONE',  ( 0.000000000000000000, 0.000000000000000000, 0.000000000000000000 ) ) ;
#2075 = CARTESIAN_POINT ( 'NONE',  ( 4.890515327186546912, 101.5721353500714059, -8.487905985326070990 ) ) ;
#2076 = DIRECTION ( 'NONE',  ( 0.000000000000000000, 0.000000000000000000, -1.000000000000000000 ) ) ;
#2077 = APPLICATION_CONTEXT ( 'automotive_design' ) ;
#2078 = CARTESIAN_POINT ( 'NONE',  ( -2.445080149700054274E-14, 46.28125000068280315, 50.00000000000000000 ) ) ;
#2079 = DIRECTION ( 'NONE',  ( 1.000000000000000000, 7.930164461608261426E-16, 0.000000000000000000 ) ) ;
#2080 = CARTESIAN_POINT ( 'NONE',  ( -15.45084971874737256, 31.60000000000000142, -47.55282581475767500 ) ) ;
#2081 = CARTESIAN_POINT ( 'NONE',  ( -46.06840506420015657, 20.00000000000000355, 19.08445694769762113 ) ) ;
#2082 = CARTESIAN_POINT ( 'NONE',  ( 30.81806926056962936, 25.22187500034139873, -42.41743335407646498 ) ) ;
#2083 = CARTESIAN_POINT ( 'NONE',  ( -0.1743114854953159432, 100.0076106038165165, 5.000000000000000000 ) ) ;
#2084 = CARTESIAN_POINT ( 'NONE',  ( -3.219174618344376363E-15, 29.49999999999999645, -52.57311121191334990 ) ) ;
#2085 = CARTESIAN_POINT ( 'NONE',  ( 49.86468353124999453, 26.95937500034139944, -16.20201782572376459 ) ) ;
#2086 = CARTESIAN_POINT ( 'NONE',  ( 49.86468353125001585, 48.75937500034140015, 16.20201782572375038 ) ) ;
#2087 = VERTEX_POINT ( 'NONE', #14850 ) ;
#2088 = PRODUCT_DEFINITION_CONTEXT ( 'detailed design', #14591, 'design' ) ;
#2089 = CARTESIAN_POINT ( 'NONE',  ( -49.86468353124999453, 25.95937500034139589, 16.20201782572377169 ) ) ;
#2090 = ORIENTED_EDGE ( 'NONE', *, *, #11787, .T. ) ;
#2091 = CARTESIAN_POINT ( 'NONE',  ( 0.000000000000000000, 267.0000000000000000, 0.000000000000000000 ) ) ;
#2092 = CARTESIAN_POINT ( 'NONE',  ( 9.631387414534489405E-15, 38.35937500034139447, 52.43083105670540789 ) ) ;
#2093 = FACE_OUTER_BOUND ( 'NONE', #8210, .T. ) ;
#2094 = CARTESIAN_POINT ( 'NONE',  ( -2.547328955960238000E-13, 34.50000000000000000, 49.99999999999999289 ) ) ;
#2095 = CARTESIAN_POINT ( 'NONE',  ( 49.99999999999999289, 44.88125000068279036, -16.24598481164532160 ) ) ;
#2096 = STYLED_ITEM ( 'NONE', ( #12300 ), #3320 ) ;
#2097 = CARTESIAN_POINT ( 'NONE',  ( 49.86468353124999453, 29.02187500034139234, -16.20201782572376459 ) ) ;
#2098 = CARTESIAN_POINT ( 'NONE',  ( -3.210462471511496205E-15, 29.35937500034139802, -52.43083105670540789 ) ) ;
#2099 = CARTESIAN_POINT ( 'NONE',  ( -49.99999999999999289, 35.89999999999999858, -16.24598481164531449 ) ) ;
#2100 = CARTESIAN_POINT ( 'NONE',  ( -49.86468353124999453, 27.82187500034139305, -16.20201782572375393 ) ) ;
#2101 = FACE_OUTER_BOUND ( 'NONE', #2518, .T. ) ;
#2102 = CARTESIAN_POINT ( 'NONE',  ( -40.34137639590981905, 47.65937500034139873, -29.30972558990011478 ) ) ;
#2103 = CARTESIAN_POINT ( 'NONE',  ( 49.86468353124999453, 41.02187500034139589, -16.20201782572376459 ) ) ;
#2104 = CARTESIAN_POINT ( 'NONE',  ( -40.34137639590981195, 20.12187500034139731, 29.30972558990012189 ) ) ;
#2105 = EDGE_LOOP ( 'NONE', ( #12917, #9731, #4558, #4173 ) ) ;
#2106 = VECTOR ( 'NONE', #5726, 1000.000000000000000 ) ;
#2107 = CARTESIAN_POINT ( 'NONE',  ( -40.34137639590981195, 42.05937500034139731, 29.30972558990012189 ) ) ;
#2108 = ORIENTED_EDGE ( 'NONE', *, *, #9058, .T. ) ;
#2109 = CARTESIAN_POINT ( 'NONE',  ( -15.45084971874736368, 26.18125000068280173, 47.55282581475768211 ) ) ;
#2110 = ORIENTED_EDGE ( 'NONE', *, *, #14122, .T. ) ;
#2111 = DIRECTION ( 'NONE',  ( 0.000000000000000000, 1.000000000000000000, 0.000000000000000000 ) ) ;
#2112 = CARTESIAN_POINT ( 'NONE',  ( -49.86468353125000164, 43.92187500034140157, 0.000000000000000000 ) ) ;
#2113 = CARTESIAN_POINT ( 'NONE',  ( -30.81806926056963292, 45.62187500034139020, -42.41743335407647209 ) ) ;
#2114 = LINE ( 'NONE', #5876, #1458 ) ;
#2115 = CARTESIAN_POINT ( 'NONE',  ( -30.81806926056962226, 26.22187500034139518, 42.41743335407647919 ) ) ;
#2116 = CARTESIAN_POINT ( 'NONE',  ( -30.90169943749474868, 33.48125000068279888, -42.53254041760200721 ) ) ;
#2117 = CARTESIAN_POINT ( 'NONE',  ( -49.86468353125000164, 41.92187500034139447, 0.000000000000000000 ) ) ;
#2118 = LINE ( 'NONE', #14917, #5932 ) ;
#2119 = ORIENTED_EDGE ( 'NONE', *, *, #7947, .T. ) ;
#2120 = CARTESIAN_POINT ( 'NONE',  ( -49.86468353125000164, 41.92187500034139447, 0.000000000000000000 ) ) ;
#2121 = CARTESIAN_POINT ( 'NONE',  ( -50.00000000000000000, 43.78125000068280315, 0.000000000000000000 ) ) ;
#2122 = ORIENTED_EDGE ( 'NONE', *, *, #13728, .T. ) ;
#2123 = ORIENTED_EDGE ( 'NONE', *, *, #4267, .F. ) ;
#2124 =( BOUNDED_SURFACE ( )  B_SPLINE_SURFACE ( 1, 2, ( 
 ( #4522, #9507, #5766, #2247, #15897, #14709, #8327, #756, #10910, #7257, #15974, #2086, #8413, #11083, #13638, #13480, #12237, #14632, #7341, #839, #10993, #10748, #584, #15806, #3179, #3256, #13391, #11246, #5101, #11478, #7660, #12563, #10155, #3594, #16304, #1327, #12410, #1082, #4940, #8653, #16392, #13964, #13725, #12731, #5181, #5025, #4857, #6419, #15295, #76, #14048, #10235, #15130, #9914, #3920, #9994, #8991, #2665, #2587, #7420, #2339, #12489, #6100, #3683, #6254, #1000, #13804, #8737, #6173, #11170, #7493, #14968, #2496, #15055, #16225, #10078, #7573, #2415, #418, #1160, #11324, #3757, #8816, #13881, #12650, #1248, #6341, #11405, #15206, #3837, #8902, #6595, #9398, #10651, #14126, #6501, #6839, #2832, #9073, #403, #324, #5350, #8061, #11649, #7739, #244, #6675, #12979, #7818, #11557, #12806, #5511, #11804, #14207, #13057, #10404, #1408, #9242, #15460, #163, #9321, #4331, #2742, #2917, #10482, #11890, #488, #4078, #13134, #1582, #1659, #5271, #15629, #1741, #14294, #10321, #5424, #15704, #9152, #12891, #7902, #6758, #2992, #15380, #11724, #15542, #4172, #7983, #14372, #10574, #4254, #1500, #4001, #5588, #14446, #3071, #13538, #5822, #15876, #12042, #10813, #8387, #5905, #2143, #4498, #9636, #8306, #10723, #9810, #3408, #10888, #5739, #7231, #816, #11056, #10966, #14689, #16031, #6914, #12289, #13372, #563, #643, #892, #14532, #12215, #5988, #9728, #4659, #11967, #15951, #14776, #8472, #16124, #4754, #9563, #8151, #3316, #1820, #9483, #13218, #5658, #13458, #1975, #13294, #15785, #14609, #2065, #4410, #3154, #8228, #1894, #7155, #6986, #3233, #7068, #12131, #737, #4573, #15186, #1135, #6319, #13939, #8714, #16449, #8625, #8545, #10055, #1059, #6078, #9969, #3658, #3490, #11300, #7641, #5081, #13779, #13697, #4832, #3570, #4915, #2313, #2221, #7398, #54, #16203, #7473, #6151, #15027, #2392, #13859, #16279, #16362, #12540, #10134, #3815, #6229, #5000, #12467, #5158, #15109, #3734, #13615, #8795, #7316, #11458, #11221, #2474, #7552, #12624, #2562, #8880, #1224, #11384, #11145, #12707, #1306, #14861, #6397, #12381, #9889, #978, #14943, #1388, #5484, #2971, #14187, #2642, #15610, #13112, #4232, #11867, #10554, #12956, #7716, #14354, #7798, #1718, #6817, #11780, #5250 ),
 ( #3900, #380, #468, #10302, #5402, #1560, #8041, #10215, #12868, #9301, #15438, #15516, #15267, #1638, #8969, #303, #14027, #7879, #12785, #14104, #11534, #10382, #4147, #6477, #135, #2805, #4057, #11628, #9127, #15359, #13035, #6654, #3978, #9050, #7962, #10460, #2719, #1474, #11704, #6570, #225, #5331, #9219, #6733, #14272, #2896, #12109, #10793, #13199, #12270, #5884, #8285, #8208, #9702, #3296, #5719, #14667, #1803, #4390, #10946, #5572, #10704, #14512, #6895, #9543, #7134, #11948, #795, #14757, #14588, #14427, #16011, #8452, #4637, #7209, #3386, #13354, #3047, #13516, #3136, #2120, #10632, #12193, #546, #5638, #15763, #15684, #13276, #15855, #4311, #6971, #1876, #9458, #9377, #623, #8124, #715, #12024, #4477, #3214, #5799, #1954, #9618, #7046, #10869, #15933, #4555, #8365, #13437, #2045, #13594, #13840, #7380, #8602, #1198, #957, #6299, #7535, #2201, #11031, #3719, #13676, #8526, #7457, #1038, #16186, #10039, #6055, #873, #11126, #12446, #2291, #12353, #16102, #6134, #3469, #15003, #15091, #7297, #3550, #9792, #4815, #4980, #14839, #11205, #9868, #14919, #9948, #16257, #4891, #3641, #8695, #13761, #4735, #2374, #5968, #8779, #12524, #1116, #6212, #11282, #16340, #2454, #12604, #9597, #5944, #852, #5780, #10846, #14567, #6029, #12169, #15910, #9431, #8342, #14481, #12329, #9520, #4534, #3191, #8429, #14815, #11007, #931, #14644, #8186, #5860, #598, #3114, #3272, #10924, #3446, #3358, #16069, #13328, #13403, #2018, #15735, #15986, #5693, #10761, #13573, #7113, #770, #4366, #8264, #13252, #2177, #15823, #1852, #8508, #4612, #4455, #13492, #9675, #1930, #4704, #7023, #6948, #12077, #14725, #2100, #683, #12002, #7188, #12249, #9768, #7273, #9022, #6450, #5134, #7520, #6621, #194, #2615, #2529, #4029, #14077, #7848, #7768, #11509, #12838, #3711, #15412, #10187, #13830, #8850, #9099, #11357, #2692, #14158, #6531, #1443, #8768, #12761, #11596, #5300, #10349, #2774, #7609, #12928, #106, #15082, #6287, #1531, #2443, #5212, #15241, #10108, #12593, #1280, #15329, #16331, #10030, #4970, #1188, #3948, #16422, #5058, #15160, #3786, #13910, #12684, #6370, #7691, #11436, #28, #3866, #8939, #13998, #1360, #10272, #14326, #2864, #6787, #440, #273, #8091, #4449, #1847, #5543 ) ),
 .UNSPECIFIED., .F., .F., .F. ) 
 B_SPLINE_SURFACE_WITH_KNOTS ( ( 2, 2 ),
 ( 3, 2, 2, 2, 2, 2, 2, 2, 2, 2, 2, 2, 2, 2, 2, 2, 2, 2, 2, 2, 2, 2, 2, 2, 2, 2, 2, 2, 2, 2, 2, 2, 2, 2, 2, 2, 2, 2, 2, 2, 2, 2, 2, 2, 2, 2, 2, 2, 2, 2, 2, 2, 2, 2, 2, 2, 2, 2, 2, 2, 2, 2, 2, 2, 2, 2, 2, 2, 2, 2, 2, 2, 2, 2, 2, 2, 2, 2, 2, 2, 2, 2, 2, 2, 2, 2, 2, 2, 2, 2, 2, 2, 2, 2, 2, 2, 2, 2, 2, 2, 2, 2, 2, 2, 2, 2, 2, 2, 2, 2, 2, 2, 2, 2, 2, 2, 2, 2, 2, 2, 2, 2, 2, 2, 2, 2, 2, 2, 2, 2, 2, 2, 2, 2, 2, 2, 2, 2, 2, 2, 2, 2, 2, 2, 2, 2, 2, 2, 2, 2, 3 ),
 ( 0.000000000000000000, 1.000000000000000000 ),
 ( 0.000000000000000000, 0.006666666666666667095, 0.01333333333333333419, 0.02000000000000000042, 0.02666666666666666838, 0.03333333333333333287, 0.04000000000000000083, 0.04666666666666666879, 0.05333333333333333676, 0.05999999999999999778, 0.06666666666666666574, 0.07333333333333333370, 0.08000000000000000167, 0.08666666666666666963, 0.09333333333333333759, 0.1000000000000000056, 0.1066666666666666735, 0.1133333333333333276, 0.1199999999999999956, 0.1266666666666666774, 0.1333333333333333315, 0.1400000000000000133, 0.1466666666666666674, 0.1533333333333333215, 0.1600000000000000033, 0.1666666666666666574, 0.1733333333333333393, 0.1799999999999999933, 0.1866666666666666752, 0.1933333333333333293, 0.2000000000000000111, 0.2066666666666666652, 0.2133333333333333470, 0.2200000000000000011, 0.2266666666666666552, 0.2333333333333333370, 0.2399999999999999911, 0.2466666666666666730, 0.2533333333333333548, 0.2600000000000000089, 0.2666666666666666630, 0.2733333333333333171, 0.2800000000000000266, 0.2866666666666666807, 0.2933333333333333348, 0.2999999999999999889, 0.3066666666666666430, 0.3133333333333333526, 0.3200000000000000067, 0.3266666666666666607, 0.3333333333333333148, 0.3400000000000000244, 0.3466666666666666785, 0.3533333333333333326, 0.3599999999999999867, 0.3666666666666666408, 0.3733333333333333504, 0.3800000000000000044, 0.3866666666666666585, 0.3933333333333333126, 0.4000000000000000222, 0.4066666666666666763, 0.4133333333333333304, 0.4199999999999999845, 0.4266666666666666941, 0.4333333333333333481, 0.4400000000000000022, 0.4466666666666666563, 0.4533333333333333104, 0.4600000000000000200, 0.4666666666666666741, 0.4733333333333333282, 0.4799999999999999822, 0.4866666666666666918, 0.4933333333333333459, 0.5000000000000000000, 0.5066666666666667096, 0.5133333333333333082, 0.5200000000000000178, 0.5266666666666666163, 0.5333333333333333259, 0.5400000000000000355, 0.5466666666666666341, 0.5533333333333333437, 0.5600000000000000533, 0.5666666666666666519, 0.5733333333333333615, 0.5799999999999999600, 0.5866666666666666696, 0.5933333333333333792, 0.5999999999999999778, 0.6066666666666666874, 0.6133333333333332860, 0.6199999999999999956, 0.6266666666666667052, 0.6333333333333333037, 0.6400000000000000133, 0.6466666666666666119, 0.6533333333333333215, 0.6600000000000000311, 0.6666666666666666297, 0.6733333333333333393, 0.6800000000000000488, 0.6866666666666666474, 0.6933333333333333570, 0.6999999999999999556, 0.7066666666666666652, 0.7133333333333333748, 0.7199999999999999734, 0.7266666666666666829, 0.7333333333333332815, 0.7399999999999999911, 0.7466666666666667007, 0.7533333333333332993, 0.7600000000000000089, 0.7666666666666667185, 0.7733333333333333171, 0.7800000000000000266, 0.7866666666666666252, 0.7933333333333333348, 0.8000000000000000444, 0.8066666666666666430, 0.8133333333333333526, 0.8199999999999999512, 0.8266666666666666607, 0.8333333333333333703, 0.8399999999999999689, 0.8466666666666666785, 0.8533333333333333881, 0.8599999999999999867, 0.8666666666666666963, 0.8733333333333332948, 0.8800000000000000044, 0.8866666666666667140, 0.8933333333333333126, 0.9000000000000000222, 0.9066666666666666208, 0.9133333333333333304, 0.9200000000000000400, 0.9266666666666666385, 0.9333333333333333481, 0.9399999999999999467, 0.9466666666666666563, 0.9533333333333333659, 0.9599999999999999645, 0.9666666666666666741, 0.9733333333333333837, 0.9799999999999999822, 0.9866666666666666918, 0.9933333333333332904, 1.000000000000000000 ),
 .UNSPECIFIED. ) 
 GEOMETRIC_REPRESENTATION_ITEM ( )  RATIONAL_B_SPLINE_SURFACE ( (
 ( 1.000000000000000000, 0.9510565162951535312, 1.000000000000000000, 0.9510565162951535312, 1.000000000000000000, 0.9510565162951535312, 1.000000000000000000, 0.9510565162951535312, 1.000000000000000000, 0.9510565162951535312, 1.000000000000000000, 0.9510565162951535312, 1.000000000000000000, 0.9510565162951535312, 1.000000000000000000, 0.9510565162951535312, 1.000000000000000000, 0.9510565162951535312, 1.000000000000000000, 0.9510565162951535312, 1.000000000000000000, 0.9510565162951535312, 1.000000000000000000, 0.9510565162951535312, 1.000000000000000000, 0.9510565162951535312, 1.000000000000000000, 0.9510565162951535312, 1.000000000000000000, 0.9510565162951535312, 1.000000000000000000, 0.9510565162951535312, 1.000000000000000000, 0.9510565162951535312, 1.000000000000000000, 0.9510565162951535312, 1.000000000000000000, 0.9510565162951535312, 1.000000000000000000, 0.9510565162951535312, 1.000000000000000000, 0.9510565162951535312, 1.000000000000000000, 0.9510565162951535312, 1.000000000000000000, 0.9510565162951535312, 1.000000000000000000, 0.9510565162951535312, 1.000000000000000000, 0.9510565162951535312, 1.000000000000000000, 0.9510565162951535312, 1.000000000000000000, 0.9510565162951535312, 1.000000000000000000, 0.9510565162951535312, 1.000000000000000000, 0.9510565162951535312, 1.000000000000000000, 0.9510565162951535312, 1.000000000000000000, 0.9510565162951535312, 1.000000000000000000, 0.9510565162951535312, 1.000000000000000000, 0.9510565162951535312, 1.000000000000000000, 0.9510565162951535312, 1.000000000000000000, 0.9510565162951535312, 1.000000000000000000, 0.9510565162951535312, 1.000000000000000000, 0.9510565162951535312, 1.000000000000000000, 0.9510565162951535312, 1.000000000000000000, 0.9510565162951535312, 1.000000000000000000, 0.9510565162951535312, 1.000000000000000000, 0.9510565162951535312, 1.000000000000000000, 0.9510565162951535312, 1.000000000000000000, 0.9510565162951535312, 1.000000000000000000, 0.9510565162951535312, 1.000000000000000000, 0.9510565162951535312, 1.000000000000000000, 0.9510565162951535312, 1.000000000000000000, 0.9510565162951535312, 1.000000000000000000, 0.9510565162951535312, 1.000000000000000000, 0.9510565162951535312, 1.000000000000000000, 0.9510565162951535312, 1.000000000000000000, 0.9510565162951535312, 1.000000000000000000, 0.9510565162951535312, 1.000000000000000000, 0.9510565162951535312, 1.000000000000000000, 0.9510565162951535312, 1.000000000000000000, 0.9510565162951535312, 1.000000000000000000, 0.9510565162951535312, 1.000000000000000000, 0.9510565162951535312, 1.000000000000000000, 0.9510565162951535312, 1.000000000000000000, 0.9510565162951535312, 1.000000000000000000, 0.9510565162951535312, 1.000000000000000000, 0.9510565162951535312, 1.000000000000000000, 0.9510565162951535312, 1.000000000000000000, 0.9510565162951535312, 1.000000000000000000, 0.9510565162951535312, 1.000000000000000000, 0.9510565162951535312, 1.000000000000000000, 0.9510565162951535312, 1.000000000000000000, 0.9510565162951535312, 1.000000000000000000, 0.9510565162951535312, 1.000000000000000000, 0.9510565162951535312, 1.000000000000000000, 0.9510565162951535312, 1.000000000000000000, 0.9510565162951535312, 1.000000000000000000, 0.9510565162951535312, 1.000000000000000000, 0.9510565162951535312, 1.000000000000000000, 0.9510565162951535312, 1.000000000000000000, 0.9510565162951535312, 1.000000000000000000, 0.9510565162951535312, 1.000000000000000000, 0.9510565162951535312, 1.000000000000000000, 0.9510565162951535312, 1.000000000000000000, 0.9510565162951535312, 1.000000000000000000, 0.9510565162951535312, 1.000000000000000000, 0.9510565162951535312, 1.000000000000000000, 0.9510565162951535312, 1.000000000000000000, 0.9510565162951535312, 1.000000000000000000, 0.9510565162951535312, 1.000000000000000000, 0.9510565162951535312, 1.000000000000000000, 0.9510565162951535312, 1.000000000000000000, 0.9510565162951535312, 1.000000000000000000, 0.9510565162951535312, 1.000000000000000000, 0.9510565162951535312, 1.000000000000000000, 0.9510565162951535312, 1.000000000000000000, 0.9510565162951535312, 1.000000000000000000, 0.9510565162951535312, 1.000000000000000000, 0.9510565162951535312, 1.000000000000000000, 0.9510565162951535312, 1.000000000000000000, 0.9510565162951535312, 1.000000000000000000, 0.9510565162951535312, 1.000000000000000000, 0.9510565162951535312, 1.000000000000000000, 0.9510565162951535312, 1.000000000000000000, 0.9510565162951535312, 1.000000000000000000, 0.9510565162951535312, 1.000000000000000000, 0.9510565162951535312, 1.000000000000000000, 0.9510565162951535312, 1.000000000000000000, 0.9510565162951535312, 1.000000000000000000, 0.9510565162951535312, 1.000000000000000000, 0.9510565162951535312, 1.000000000000000000, 0.9510565162951535312, 1.000000000000000000, 0.9510565162951535312, 1.000000000000000000, 0.9510565162951535312, 1.000000000000000000, 0.9510565162951535312, 1.000000000000000000, 0.9510565162951535312, 1.000000000000000000, 0.9510565162951535312, 1.000000000000000000, 0.9510565162951535312, 1.000000000000000000, 0.9510565162951535312, 1.000000000000000000, 0.9510565162951535312, 1.000000000000000000, 0.9510565162951535312, 1.000000000000000000, 0.9510565162951535312, 1.000000000000000000, 0.9510565162951535312, 1.000000000000000000, 0.9510565162951535312, 1.000000000000000000, 0.9510565162951535312, 1.000000000000000000, 0.9510565162951535312, 1.000000000000000000, 0.9510565162951535312, 1.000000000000000000, 0.9510565162951535312, 1.000000000000000000, 0.9510565162951535312, 1.000000000000000000, 0.9510565162951535312, 1.000000000000000000, 0.9510565162951535312, 1.000000000000000000, 0.9510565162951535312, 1.000000000000000000, 0.9510565162951535312, 1.000000000000000000, 0.9510565162951535312, 1.000000000000000000, 0.9510565162951535312, 1.000000000000000000, 0.9510565162951535312, 1.000000000000000000, 0.9510565162951535312, 1.000000000000000000, 0.9510565162951535312, 1.000000000000000000, 0.9510565162951535312, 1.000000000000000000, 0.9510565162951535312, 1.000000000000000000, 0.9510565162951535312, 1.000000000000000000, 0.9510565162951535312, 1.000000000000000000, 0.9510565162951535312, 1.000000000000000000, 0.9510565162951535312, 1.000000000000000000, 0.9510565162951535312, 1.000000000000000000, 0.9510565162951535312, 1.000000000000000000, 0.9510565162951535312, 1.000000000000000000, 0.9510565162951535312, 1.000000000000000000, 0.9510565162951535312, 1.000000000000000000, 0.9510565162951535312, 1.000000000000000000, 0.9510565162951535312, 1.000000000000000000, 0.9510565162951535312, 1.000000000000000000, 0.9510565162951535312, 1.000000000000000000, 0.9510565162951535312, 1.000000000000000000, 0.9510565162951535312, 1.000000000000000000, 0.9510565162951535312, 1.000000000000000000),
 ( 1.000000000000000000, 0.9510565162951535312, 1.000000000000000000, 0.9510565162951535312, 1.000000000000000000, 0.9510565162951535312, 1.000000000000000000, 0.9510565162951535312, 1.000000000000000000, 0.9510565162951535312, 1.000000000000000000, 0.9510565162951535312, 1.000000000000000000, 0.9510565162951535312, 1.000000000000000000, 0.9510565162951535312, 1.000000000000000000, 0.9510565162951535312, 1.000000000000000000, 0.9510565162951535312, 1.000000000000000000, 0.9510565162951535312, 1.000000000000000000, 0.9510565162951535312, 1.000000000000000000, 0.9510565162951535312, 1.000000000000000000, 0.9510565162951535312, 1.000000000000000000, 0.9510565162951535312, 1.000000000000000000, 0.9510565162951535312, 1.000000000000000000, 0.9510565162951535312, 1.000000000000000000, 0.9510565162951535312, 1.000000000000000000, 0.9510565162951535312, 1.000000000000000000, 0.9510565162951535312, 1.000000000000000000, 0.9510565162951535312, 1.000000000000000000, 0.9510565162951535312, 1.000000000000000000, 0.9510565162951535312, 1.000000000000000000, 0.9510565162951535312, 1.000000000000000000, 0.9510565162951535312, 1.000000000000000000, 0.9510565162951535312, 1.000000000000000000, 0.9510565162951535312, 1.000000000000000000, 0.9510565162951535312, 1.000000000000000000, 0.9510565162951535312, 1.000000000000000000, 0.9510565162951535312, 1.000000000000000000, 0.9510565162951535312, 1.000000000000000000, 0.9510565162951535312, 1.000000000000000000, 0.9510565162951535312, 1.000000000000000000, 0.9510565162951535312, 1.000000000000000000, 0.9510565162951535312, 1.000000000000000000, 0.9510565162951535312, 1.000000000000000000, 0.9510565162951535312, 1.000000000000000000, 0.9510565162951535312, 1.000000000000000000, 0.9510565162951535312, 1.000000000000000000, 0.9510565162951535312, 1.000000000000000000, 0.9510565162951535312, 1.000000000000000000, 0.9510565162951535312, 1.000000000000000000, 0.9510565162951535312, 1.000000000000000000, 0.9510565162951535312, 1.000000000000000000, 0.9510565162951535312, 1.000000000000000000, 0.9510565162951535312, 1.000000000000000000, 0.9510565162951535312, 1.000000000000000000, 0.9510565162951535312, 1.000000000000000000, 0.9510565162951535312, 1.000000000000000000, 0.9510565162951535312, 1.000000000000000000, 0.9510565162951535312, 1.000000000000000000, 0.9510565162951535312, 1.000000000000000000, 0.9510565162951535312, 1.000000000000000000, 0.9510565162951535312, 1.000000000000000000, 0.9510565162951535312, 1.000000000000000000, 0.9510565162951535312, 1.000000000000000000, 0.9510565162951535312, 1.000000000000000000, 0.9510565162951535312, 1.000000000000000000, 0.9510565162951535312, 1.000000000000000000, 0.9510565162951535312, 1.000000000000000000, 0.9510565162951535312, 1.000000000000000000, 0.9510565162951535312, 1.000000000000000000, 0.9510565162951535312, 1.000000000000000000, 0.9510565162951535312, 1.000000000000000000, 0.9510565162951535312, 1.000000000000000000, 0.9510565162951535312, 1.000000000000000000, 0.9510565162951535312, 1.000000000000000000, 0.9510565162951535312, 1.000000000000000000, 0.9510565162951535312, 1.000000000000000000, 0.9510565162951535312, 1.000000000000000000, 0.9510565162951535312, 1.000000000000000000, 0.9510565162951535312, 1.000000000000000000, 0.9510565162951535312, 1.000000000000000000, 0.9510565162951535312, 1.000000000000000000, 0.9510565162951535312, 1.000000000000000000, 0.9510565162951535312, 1.000000000000000000, 0.9510565162951535312, 1.000000000000000000, 0.9510565162951535312, 1.000000000000000000, 0.9510565162951535312, 1.000000000000000000, 0.9510565162951535312, 1.000000000000000000, 0.9510565162951535312, 1.000000000000000000, 0.9510565162951535312, 1.000000000000000000, 0.9510565162951535312, 1.000000000000000000, 0.9510565162951535312, 1.000000000000000000, 0.9510565162951535312, 1.000000000000000000, 0.9510565162951535312, 1.000000000000000000, 0.9510565162951535312, 1.000000000000000000, 0.9510565162951535312, 1.000000000000000000, 0.9510565162951535312, 1.000000000000000000, 0.9510565162951535312, 1.000000000000000000, 0.9510565162951535312, 1.000000000000000000, 0.9510565162951535312, 1.000000000000000000, 0.9510565162951535312, 1.000000000000000000, 0.9510565162951535312, 1.000000000000000000, 0.9510565162951535312, 1.000000000000000000, 0.9510565162951535312, 1.000000000000000000, 0.9510565162951535312, 1.000000000000000000, 0.9510565162951535312, 1.000000000000000000, 0.9510565162951535312, 1.000000000000000000, 0.9510565162951535312, 1.000000000000000000, 0.9510565162951535312, 1.000000000000000000, 0.9510565162951535312, 1.000000000000000000, 0.9510565162951535312, 1.000000000000000000, 0.9510565162951535312, 1.000000000000000000, 0.9510565162951535312, 1.000000000000000000, 0.9510565162951535312, 1.000000000000000000, 0.9510565162951535312, 1.000000000000000000, 0.9510565162951535312, 1.000000000000000000, 0.9510565162951535312, 1.000000000000000000, 0.9510565162951535312, 1.000000000000000000, 0.9510565162951535312, 1.000000000000000000, 0.9510565162951535312, 1.000000000000000000, 0.9510565162951535312, 1.000000000000000000, 0.9510565162951535312, 1.000000000000000000, 0.9510565162951535312, 1.000000000000000000, 0.9510565162951535312, 1.000000000000000000, 0.9510565162951535312, 1.000000000000000000, 0.9510565162951535312, 1.000000000000000000, 0.9510565162951535312, 1.000000000000000000, 0.9510565162951535312, 1.000000000000000000, 0.9510565162951535312, 1.000000000000000000, 0.9510565162951535312, 1.000000000000000000, 0.9510565162951535312, 1.000000000000000000, 0.9510565162951535312, 1.000000000000000000, 0.9510565162951535312, 1.000000000000000000, 0.9510565162951535312, 1.000000000000000000, 0.9510565162951535312, 1.000000000000000000, 0.9510565162951535312, 1.000000000000000000, 0.9510565162951535312, 1.000000000000000000, 0.9510565162951535312, 1.000000000000000000, 0.9510565162951535312, 1.000000000000000000, 0.9510565162951535312, 1.000000000000000000, 0.9510565162951535312, 1.000000000000000000, 0.9510565162951535312, 1.000000000000000000, 0.9510565162951535312, 1.000000000000000000, 0.9510565162951535312, 1.000000000000000000, 0.9510565162951535312, 1.000000000000000000, 0.9510565162951535312, 1.000000000000000000, 0.9510565162951535312, 1.000000000000000000, 0.9510565162951535312, 1.000000000000000000, 0.9510565162951535312, 1.000000000000000000, 0.9510565162951535312, 1.000000000000000000, 0.9510565162951535312, 1.000000000000000000, 0.9510565162951535312, 1.000000000000000000, 0.9510565162951535312, 1.000000000000000000, 0.9510565162951535312, 1.000000000000000000, 0.9510565162951535312, 1.000000000000000000, 0.9510565162951535312, 1.000000000000000000, 0.9510565162951535312, 1.000000000000000000, 0.9510565162951535312, 1.000000000000000000) ) ) 
 REPRESENTATION_ITEM ( '' )  SURFACE ( )  );
#2125 = EDGE_CURVE ( 'NONE', #404, #7781, #14519, .T. ) ;
#2126 = ORIENTED_EDGE ( 'NONE', *, *, #13766, .F. ) ;
#2127 = CARTESIAN_POINT ( 'NONE',  ( -5.000000000000000000, 96.75198296766780004, 7.580410092413951695 ) ) ;
#2128 = CARTESIAN_POINT ( 'NONE',  ( 2.600676159226421000E-13, 33.49999999999999289, -49.99999999999999289 ) ) ;
#2129 = CARTESIAN_POINT ( 'NONE',  ( -30.90169943749474513, 49.70000000000000284, -42.53254041760200721 ) ) ;
#2130 = CARTESIAN_POINT ( 'NONE',  ( 30.90169943749473802, 37.08125000068280031, -42.53254041760200721 ) ) ;
#2131 = CARTESIAN_POINT ( 'NONE',  ( -3.210462471511496205E-15, 37.35937500034139447, -52.43083105670540789 ) ) ;
#2132 = CARTESIAN_POINT ( 'NONE',  ( -49.86468353124999453, 47.95937500034138878, 16.20201782572377169 ) ) ;
#2133 = CARTESIAN_POINT ( 'NONE',  ( 7.919222016226693306, 24.55125428154684286, 50.00000000000003553 ) ) ;
#2134 = ADVANCED_FACE ( 'NONE', ( #14764 ), #13445, .F. ) ;
#2135 = ADVANCED_FACE ( 'NONE', ( #7219 ), #8534, .F. ) ;
#2136 = CARTESIAN_POINT ( 'NONE',  ( -9.642970592016617104, 101.1563493904846780, 1.872989114519528986 ) ) ;
#2137 = FACE_BOUND ( 'NONE', #5513, .T. ) ;
#2138 = DIRECTION ( 'NONE',  ( -0.000000000000000000, 1.000000000000000000, -0.000000000000000000 ) ) ;
#2139 = EDGE_CURVE ( 'NONE', #13613, #10886, #15084, .T. ) ;
#2140 = CARTESIAN_POINT ( 'NONE',  ( -0.4999999999999990563, 31.99999999999998579, 101.0000000000000000 ) ) ;
#2141 = CARTESIAN_POINT ( 'NONE',  ( -3.111920190527341144E-15, 25.28125000068279604, -50.00000000000000000 ) ) ;
#2142 = ORIENTED_EDGE ( 'NONE', *, *, #4336, .F. ) ;
#2143 = CARTESIAN_POINT ( 'NONE',  ( -30.81806926056963292, 33.55937500034138310, -42.41743335407647209 ) ) ;
#2144 = ORIENTED_EDGE ( 'NONE', *, *, #2862, .F. ) ;
#2145 = ORIENTED_EDGE ( 'NONE', *, *, #8837, .T. ) ;
#2146 = ORIENTED_EDGE ( 'NONE', *, *, #10006, .T. ) ;
#2147 = CARTESIAN_POINT ( 'NONE',  ( 15.45084971874737789, 46.38125000068279746, 47.55282581475767500 ) ) ;
#2148 = CARTESIAN_POINT ( 'NONE',  ( -30.90169943749473447, 40.30000000000000426, 42.53254041760200721 ) ) ;
#2149 = CARTESIAN_POINT ( 'NONE',  ( 2.978552182361884590E-14, 47.28125000068279604, -50.00000000000000000 ) ) ;
#2150 = ORIENTED_EDGE ( 'NONE', *, *, #15029, .F. ) ;
#2151 = DIRECTION ( 'NONE',  ( 0.000000000000000000, 1.000000000000000000, 0.000000000000000000 ) ) ;
#2152 = DIRECTION ( 'NONE',  ( 0.5877852522924688072, 0.8090169943749505599, 0.000000000000000000 ) ) ;
#2153 = CARTESIAN_POINT ( 'NONE',  ( -30.90169943749473447, 20.30000000000000071, 42.53254041760200721 ) ) ;
#2154 = CARTESIAN_POINT ( 'NONE',  ( -2.500000000000000000, 247.0000000000000284, 40.00000000000000000 ) ) ;
#2155 = DIRECTION ( 'NONE',  ( 0.000000000000000000, 0.000000000000000000, 1.000000000000000000 ) ) ;
#2156 = FACE_OUTER_BOUND ( 'NONE', #8589, .T. ) ;
#2157 = CYLINDRICAL_SURFACE ( 'NONE', #10270, 50.00000000000000000 ) ;
#2158 = CARTESIAN_POINT ( 'NONE',  ( 0.000000000000000000, 0.000000000000000000, 0.000000000000000000 ) ) ;
#2159 = CARTESIAN_POINT ( 'NONE',  ( -45.18727525474225359, 20.00000000000001066, 21.08615623785947690 ) ) ;
#2160 = CARTESIAN_POINT ( 'NONE',  ( -49.99999999999999289, 47.68125000068280173, -16.24598481164531449 ) ) ;
#2161 = DIRECTION ( 'NONE',  ( 0.000000000000000000, -1.000000000000000000, 0.000000000000000000 ) ) ;
#2162 = CARTESIAN_POINT ( 'NONE',  ( -15.45084971874736368, 28.40000000000000213, 47.55282581475768211 ) ) ;
#2163 = CARTESIAN_POINT ( 'NONE',  ( 30.81806926056962936, 27.15937500034139163, -42.41743335407647209 ) ) ;
#2164 = DIRECTION ( 'NONE',  ( 1.000000000000000000, 0.000000000000000000, 0.000000000000000000 ) ) ;
#2165 = ORIENTED_EDGE ( 'NONE', *, *, #6538, .F. ) ;
#2166 = CARTESIAN_POINT ( 'NONE',  ( 9.485510086921706829, 8.593664601562213790, 101.6666710451724214 ) ) ;
#2167 = ORIENTED_EDGE ( 'NONE', *, *, #2746, .F. ) ;
#2168 =( REPRESENTATION_RELATIONSHIP ('NONE','NONE', #6178, #15829 ) REPRESENTATION_RELATIONSHIP_WITH_TRANSFORMATION ( #867 )SHAPE_REPRESENTATION_RELATIONSHIP( ) );
#2169 = LINE ( 'NONE', #12241, #956 ) ;
#2170 = CARTESIAN_POINT ( 'NONE',  ( 15.40903463028482356, 34.45937500034139589, 47.42413220539093999 ) ) ;
#2171 = DIRECTION ( 'NONE',  ( -0.3090169943749448422, -0.9510565162951544194, 0.000000000000000000 ) ) ;
#2172 = CARTESIAN_POINT ( 'NONE',  ( -30.27664397204038593, 25.00000000000000355, 26.14048258526057467 ) ) ;
#2173 = LINE ( 'NONE', #13488, #9734 ) ;
#2174 = CARTESIAN_POINT ( 'NONE',  ( 30.81806926056964002, 28.62187500034140086, 42.41743335407647209 ) ) ;
#2175 = CARTESIAN_POINT ( 'NONE',  ( -49.86468353125000164, 27.85937500034139447, 0.000000000000000000 ) ) ;
#2176 = CARTESIAN_POINT ( 'NONE',  ( -1.240322475938754499E-13, 36.50000000000000711, 50.00000000000000000 ) ) ;
#2177 = CARTESIAN_POINT ( 'NONE',  ( 30.81806926056962936, 29.22187500034139873, -42.41743335407647209 ) ) ;
#2178 = FACE_OUTER_BOUND ( 'NONE', #5573, .T. ) ;
#2179 = CARTESIAN_POINT ( 'NONE',  ( 40.34137639590981905, 46.65937500034139873, 29.30972558990010768 ) ) ;
#2180 = CARTESIAN_POINT ( 'NONE',  ( 40.34137639590981905, 36.72187500034139163, 29.30972558990010768 ) ) ;
#2181 = CIRCLE ( 'NONE', #10438, 5.000000000000000000 ) ;
#2182 = CARTESIAN_POINT ( 'NONE',  ( 15.40903463028482356, 22.52187500034139589, 47.42413220539093999 ) ) ;
#2183 = EDGE_CURVE ( 'NONE', #891, #12043, #14013, .T. ) ;
#2184 = ORIENTED_EDGE ( 'NONE', *, *, #1684, .F. ) ;
#2185 = CARTESIAN_POINT ( 'NONE',  ( -49.86468353124999453, 43.75937500034140015, -16.20201782572375393 ) ) ;
#2186 = ORIENTED_EDGE ( 'NONE', *, *, #8364, .F. ) ;
#2187 = CARTESIAN_POINT ( 'NONE',  ( -15.45084971874737256, 23.38125000068280102, -47.55282581475767500 ) ) ;
#2188 = ORIENTED_EDGE ( 'NONE', *, *, #9653, .T. ) ;
#2189 = AXIS2_PLACEMENT_3D ( 'NONE', #14664, #8362, #10630 ) ;
#2190 = DIRECTION ( 'NONE',  ( -5.069245582283711292E-17, -1.000000000000000000, 8.780190904559502465E-17 ) ) ;
#2191 = CARTESIAN_POINT ( 'NONE',  ( -15.40903463028480580, 36.32187500034140015, 47.42413220539094709 ) ) ;
#2192 = CARTESIAN_POINT ( 'NONE',  ( -49.86468353124999453, 48.02187500034139589, 16.20201782572377525 ) ) ;
#2193 = CARTESIAN_POINT ( 'NONE',  ( -20.00000000000000355, 307.0000000000000568, -2.499999999999998668 ) ) ;
#2194 = CARTESIAN_POINT ( 'NONE',  ( 15.40903463028481113, 25.32187500034139660, -47.42413220539094709 ) ) ;
#2195 = ITEM_DEFINED_TRANSFORMATION ( 'NONE', 'NONE', #2811,  #15812 ) ;
#2196 = CARTESIAN_POINT ( 'NONE',  ( 15.45084971874736723, 35.18125000068280173, -47.55282581475768211 ) ) ;
#2197 = CARTESIAN_POINT ( 'NONE',  ( 49.86468353124999453, 39.02187500034138878, -16.20201782572376459 ) ) ;
#2198 = CARTESIAN_POINT ( 'NONE',  ( -26.69586624682724718, 283.2330659413073590, -5.891732493678455640 ) ) ;
#2199 = ORIENTED_EDGE ( 'NONE', *, *, #716, .T. ) ;
#2200 = VECTOR ( 'NONE', #9579, 1000.000000000000227 ) ;
#2201 = CARTESIAN_POINT ( 'NONE',  ( -40.34137639590981195, 38.12187500034139731, 29.30972558990012189 ) ) ;
#2202 = CARTESIAN_POINT ( 'NONE',  ( -15.45084971874737256, 31.38125000068280102, -47.55282581475767500 ) ) ;
#2203 = ORIENTED_EDGE ( 'NONE', *, *, #13732, .T. ) ;
#2204 = ORIENTED_EDGE ( 'NONE', *, *, #5294, .T. ) ;
#2205 = ORIENTED_EDGE ( 'NONE', *, *, #199, .F. ) ;
#2206 = CARTESIAN_POINT ( 'NONE',  ( -30.90169943749473447, 40.08125000068279320, 42.53254041760200721 ) ) ;
#2207 = CARTESIAN_POINT ( 'NONE',  ( 12.16951863902660236, 34.13030016454095517, 101.6666710451724214 ) ) ;
#2208 = FACE_BOUND ( 'NONE', #695, .T. ) ;
#2209 = CARTESIAN_POINT ( 'NONE',  ( 0.000000000000000000, 20.00000000000000355, 0.000000000000000000 ) ) ;
#2210 = CARTESIAN_POINT ( 'NONE',  ( -49.86468353124999453, 39.75937500034139305, -16.20201782572375393 ) ) ;
#2211 = CARTESIAN_POINT ( 'NONE',  ( -49.86468353124999453, 47.75937500034139305, -16.20201782572375393 ) ) ;
#2212 = LINE ( 'NONE', #15943, #10347 ) ;
#2213 = AXIS2_PLACEMENT_3D ( 'NONE', #13775, #1302, #15180 ) ;
#2214 = PLANE ( 'NONE',  #15033 ) ;
#2215 = CARTESIAN_POINT ( 'NONE',  ( 7.580410092413973011, 102.0000000000000142, 5.000000000000000000 ) ) ;
#2216 = EDGE_CURVE ( 'NONE', #9078, #10576, #10369, .T. ) ;
#2217 = CARTESIAN_POINT ( 'NONE',  ( -3.111920190527341144E-15, 43.28125000068280315, -50.00000000000000000 ) ) ;
#2218 = DIRECTION ( 'NONE',  ( 0.000000000000000000, -1.000000000000000000, 0.000000000000000000 ) ) ;
#2219 = ORIENTED_EDGE ( 'NONE', *, *, #7014, .F. ) ;
#2220 =( BOUNDED_CURVE ( )  B_SPLINE_CURVE ( 2, ( #15889, #7001, #5757, #3332, #4512, #8242, #10826, #2239, #14876, #831, #14623, #12056, #6003 ),
 .UNSPECIFIED., .F., .T. ) 
 B_SPLINE_CURVE_WITH_KNOTS ( ( 3, 2, 2, 2, 2, 2, 3 ),
 ( 0.05000000000000000278, 0.05333333333333333676, 0.05999999999999999778, 0.06666666666666666574, 0.07333333333333333370, 0.08000000000000000167, 0.08333333333333334259 ),
 .UNSPECIFIED. ) 
 CURVE ( )  GEOMETRIC_REPRESENTATION_ITEM ( )  RATIONAL_B_SPLINE_CURVE ( ( 0.9755282581475768211, 0.9755282581475768211, 1.000000000000000000, 0.9510565162951535312, 1.000000000000000000, 0.9510565162951535312, 1.000000000000000000, 0.9510565162951535312, 1.000000000000000000, 0.9510565162951535312, 1.000000000000000000, 0.9755282581475767101, 0.9755282581475768211 ) ) 
 REPRESENTATION_ITEM ( '' )  );
#2221 = CARTESIAN_POINT ( 'NONE',  ( -40.34137639590981905, 25.65937500034139518, -29.30972558990011478 ) ) ;
#2222 = EDGE_LOOP ( 'NONE', ( #11670, #9442, #4893 ) ) ;
#2223 = EDGE_CURVE ( 'NONE', #6735, #758, #10126, .T. ) ;
#2224 = VERTEX_POINT ( 'NONE', #2382 ) ;
#2225 = VERTEX_POINT ( 'NONE', #2632 ) ;
#2226 = EDGE_CURVE ( 'NONE', #4835, #13275, #13753, .T. ) ;
#2227 = VECTOR ( 'NONE', #6565, 1000.000000000000114 ) ;
#2228 = CARTESIAN_POINT ( 'NONE',  ( 40.45084971874737079, 40.98125000068279888, -29.38926261462366440 ) ) ;
#2229 = DIRECTION ( 'NONE',  ( 0.000000000000000000, 1.000000000000000000, 0.000000000000000000 ) ) ;
#2230 = CARTESIAN_POINT ( 'NONE',  ( 6.123233995736766085E-15, 193.4213562373095385, 50.00000000000000000 ) ) ;
#2231 = ORIENTED_EDGE ( 'NONE', *, *, #7880, .T. ) ;
#2232 = CARTESIAN_POINT ( 'NONE',  ( 5.510910596163090344E-15, 267.0000000000000000, 45.00000000000000711 ) ) ;
#2233 = CARTESIAN_POINT ( 'NONE',  ( -15.45084971874736368, 28.18125000068279817, 47.55282581475768211 ) ) ;
#2234 = ADVANCED_FACE ( 'NONE', ( #9878 ), #7627, .F. ) ;
#2235 = CARTESIAN_POINT ( 'NONE',  ( -13.93607900078482054, 11.90003901379968632, 96.90546041726973669 ) ) ;
#2236 = CARTESIAN_POINT ( 'NONE',  ( -15.84787772126911776, 28.17501872725009093, 101.6666710451724214 ) ) ;
#2237 = CARTESIAN_POINT ( 'NONE',  ( -25.00000000000000355, 312.0000000000000568, -7.499999999999999112 ) ) ;
#2238 = DIRECTION ( 'NONE',  ( 0.8090169943749426773, 0.5877852522924797984, 0.000000000000000000 ) ) ;
#2239 = CARTESIAN_POINT ( 'NONE',  ( -49.99999999999999289, 47.89999999999999858, -16.24598481164531449 ) ) ;
#2240 = CARTESIAN_POINT ( 'NONE',  ( 15.45084971874737789, 46.60000000000000142, 47.55282581475767500 ) ) ;
#2241 = CARTESIAN_POINT ( 'NONE',  ( 37.77664397204061686, 25.00000000000000355, 13.15010152849349900 ) ) ;
#2242 = CARTESIAN_POINT ( 'NONE',  ( -49.99999999999999289, 43.88125000068279746, 16.24598481164533226 ) ) ;
#2243 = DIRECTION ( 'NONE',  ( 0.000000000000000000, 0.000000000000000000, -1.000000000000000000 ) ) ;
#2244 = VECTOR ( 'NONE', #12631, 1000.000000000000000 ) ;
#2245 = EDGE_CURVE ( 'NONE', #14735, #12589, #14929, .T. ) ;
#2246 = CARTESIAN_POINT ( 'NONE',  ( 50.00000000000000711, 26.89999999999999503, 16.24598481164530739 ) ) ;
#2247 = CARTESIAN_POINT ( 'NONE',  ( -30.81806926056963292, 49.55937500034139731, -42.41743335407647209 ) ) ;
#2248 = ORIENTED_EDGE ( 'NONE', *, *, #9105, .T. ) ;
#2249 = CARTESIAN_POINT ( 'NONE',  ( 9.681523229999685398, 8.323875655254958872, 101.3333374614808662 ) ) ;
#2250 = VERTEX_POINT ( 'NONE', #7390 ) ;
#2251 = DIRECTION ( 'NONE',  ( -0.000000000000000000, -1.000000000000000000, -0.000000000000000000 ) ) ;
#2252 = CARTESIAN_POINT ( 'NONE',  ( -49.86468353125000164, 37.85937500034139447, 0.000000000000000000 ) ) ;
#2253 = VECTOR ( 'NONE', #11449, 1000.000000000000114 ) ;
#2254 = EDGE_CURVE ( 'NONE', #7234, #12941, #8612, .T. ) ;
#2255 = CARTESIAN_POINT ( 'NONE',  ( 15.45084971874737789, 40.38125000068280457, 47.55282581475767500 ) ) ;
#2256 = CYLINDRICAL_SURFACE ( 'NONE', #3615, 5.000000000000000000 ) ;
#2257 = CARTESIAN_POINT ( 'NONE',  ( 2.600676159226421000E-13, 31.28125000068279604, -49.99999999999999289 ) ) ;
#2258 = CARTESIAN_POINT ( 'NONE',  ( 50.00000000000000711, 44.68125000068278752, 16.24598481164530739 ) ) ;
#2259 = CARTESIAN_POINT ( 'NONE',  ( 49.86468353124999453, 23.02187500034139944, -16.20201782572376459 ) ) ;
#2260 = CARTESIAN_POINT ( 'NONE',  ( -15.40903463028480580, 30.25937500034140015, 47.42413220539094709 ) ) ;
#2261 = DIRECTION ( 'NONE',  ( -1.000000000000000000, 0.000000000000000000, 0.000000000000000000 ) ) ;
#2262 = CARTESIAN_POINT ( 'NONE',  ( 40.34137639590981905, 36.72187500034139163, 29.30972558990010768 ) ) ;
#2263 = EDGE_CURVE ( 'NONE', #5800, #1641, #12454, .T. ) ;
#2264 = CARTESIAN_POINT ( 'NONE',  ( -0.5000000000000000000, 244.0000000000000284, -49.99999999999999289 ) ) ;
#2265 = CARTESIAN_POINT ( 'NONE',  ( 49.86468353125001585, 36.75937500034138594, 16.20201782572375038 ) ) ;
#2266 = CARTESIAN_POINT ( 'NONE',  ( -15.40903463028481646, 35.52187500034139589, -47.42413220539093999 ) ) ;
#2267 = AXIS2_PLACEMENT_3D ( 'NONE', #7, #12739, #12815 ) ;
#2268 = CARTESIAN_POINT ( 'NONE',  ( -30.90169943749474868, 45.70000000000000995, -42.53254041760200721 ) ) ;
#2269 = APPLICATION_CONTEXT ( 'automotive_design' ) ;
#2270 = MECHANICAL_DESIGN_GEOMETRIC_PRESENTATION_REPRESENTATION (  '', ( #7583 ), #14469 ) ;
#2271 = VERTEX_POINT ( 'NONE', #5149 ) ;
#2272 = CARTESIAN_POINT ( 'NONE',  ( 49.86468353124999453, 40.95937500034140299, -16.20201782572376104 ) ) ;
#2273 = VERTEX_POINT ( 'NONE', #6220 ) ;
#2274 = EDGE_CURVE ( 'NONE', #11502, #11404, #12970, .T. ) ;
#2275 = CARTESIAN_POINT ( 'NONE',  ( -50.00000000000000000, 23.78125000068279959, 0.000000000000000000 ) ) ;
#2276 = ORIENTED_EDGE ( 'NONE', *, *, #6208, .T. ) ;
#2277 = VECTOR ( 'NONE', #16147, 1000.000000000000000 ) ;
#2278 = AXIS2_PLACEMENT_3D ( 'NONE', #11213, #11289, #3478 ) ;
#2279 = AXIS2_PLACEMENT_3D ( 'NONE', #1623, #4606, #2010 ) ;
#2280 = CIRCLE ( 'NONE', #5231, 17.50000000000000000 ) ;
#2281 = CARTESIAN_POINT ( 'NONE',  ( 7.919222016226875382, 41.22999571913594963, -49.99999999999997158 ) ) ;
#2282 = CARTESIAN_POINT ( 'NONE',  ( 30.81806926056962936, 47.22187500034139873, -42.41743335407647209 ) ) ;
#2283 = CARTESIAN_POINT ( 'NONE',  ( 50.00000000000000711, 30.89999999999999858, 16.24598481164530739 ) ) ;
#2284 = CARTESIAN_POINT ( 'NONE',  ( 49.86468353124999453, 23.02187500034139944, -16.20201782572376459 ) ) ;
#2285 = CARTESIAN_POINT ( 'NONE',  ( -15.45084971874737256, 35.38125000068279746, -47.55282581475767500 ) ) ;
#2286 = CARTESIAN_POINT ( 'NONE',  ( 49.86468353125001585, 36.82187500034140015, 16.20201782572375038 ) ) ;
#2287 = CARTESIAN_POINT ( 'NONE',  ( -29.34549410641294287, 282.0000000000000000, -12.17274705320727080 ) ) ;
#2288 = AXIS2_PLACEMENT_3D ( 'NONE', #1926, #4787, #14563 ) ;
#2289 = AXIS2_PLACEMENT_3D ( 'NONE', #2983, #4908, #8616 ) ;
#2290 = AXIS2_PLACEMENT_3D ( 'NONE', #12049, #5593, #648 ) ;
#2291 = CARTESIAN_POINT ( 'NONE',  ( 49.86468353125001585, 36.82187500034140015, 16.20201782572375038 ) ) ;
#2292 = CARTESIAN_POINT ( 'NONE',  ( -8.880528407616480990, 25.91118970470954963, 101.0000000000000000 ) ) ;
#2293 = ORIENTED_EDGE ( 'NONE', *, *, #6374, .T. ) ;
#2294 = ORIENTED_EDGE ( 'NONE', *, *, #3693, .F. ) ;
#2295 = EDGE_LOOP ( 'NONE', ( #3961, #2144 ) ) ;
#2296 = DIRECTION ( 'NONE',  ( -0.000000000000000000, 1.000000000000000000, 0.000000000000000000 ) ) ;
#2297 = CARTESIAN_POINT ( 'NONE',  ( -3.407225380398804404, 31.38205016914259105, 102.0000000000000142 ) ) ;
#2298 = CARTESIAN_POINT ( 'NONE',  ( -50.00000000000000000, 21.78125000068279959, 0.000000000000000000 ) ) ;
#2299 = CARTESIAN_POINT ( 'NONE',  ( -49.99999999999999289, 23.88125000068279746, 16.24598481164533226 ) ) ;
#2300 = AXIS2_PLACEMENT_3D ( 'NONE', #9631, #13368, #2061 ) ;
#2301 = ADVANCED_FACE ( 'NONE', ( #4900 ), #15014, .F. ) ;
#2302 = VECTOR ( 'NONE', #90, 1000.000000000000000 ) ;
#2303 = CARTESIAN_POINT ( 'NONE',  ( -3.210462471511496205E-15, 39.35937500034138736, -52.43083105670540789 ) ) ;
#2304 = CARTESIAN_POINT ( 'NONE',  ( -49.86468353124999453, 41.95937500034139589, 16.20201782572377169 ) ) ;
#2305 = CARTESIAN_POINT ( 'NONE',  ( 0.000000000000000000, 242.0000000000000284, 45.00000000000000000 ) ) ;
#2306 = AXIS2_PLACEMENT_3D ( 'NONE', #10308, #1481, #141 ) ;
#2307 = AXIS2_PLACEMENT_3D ( 'NONE', #15891, #14625, #3251 ) ;
#2308 = CARTESIAN_POINT ( 'NONE',  ( 0.000000000000000000, 242.0000000000000284, 0.000000000000000000 ) ) ;
#2309 = CIRCLE ( 'NONE', #14787, 6.000000000000001776 ) ;
#2310 = CARTESIAN_POINT ( 'NONE',  ( 30.90169943749473802, 43.08125000068280031, -42.53254041760200721 ) ) ;
#2311 = CARTESIAN_POINT ( 'NONE',  ( -50.00000000000000000, 42.00000000000000000, 0.000000000000000000 ) ) ;
#2312 = VERTEX_POINT ( 'NONE', #3727 ) ;
#2313 = CARTESIAN_POINT ( 'NONE',  ( -49.86468353124999453, 25.75937500034140015, -16.20201782572375393 ) ) ;
#2314 = EDGE_CURVE ( 'NONE', #761, #12474, #1282, .T. ) ;
#2315 = CARTESIAN_POINT ( 'NONE',  ( -50.00000000000000000, 47.78125000068279604, 0.000000000000000000 ) ) ;
#2316 = ORIENTED_EDGE ( 'NONE', *, *, #14670, .T. ) ;
#2317 = ORIENTED_EDGE ( 'NONE', *, *, #6640, .F. ) ;
#2318 = CARTESIAN_POINT ( 'NONE',  ( 15.45084971874737789, 36.38125000068279746, 47.55282581475767500 ) ) ;
#2319 = CARTESIAN_POINT ( 'NONE',  ( 50.00000000000000711, 46.90000000000000568, 16.24598481164530739 ) ) ;
#2320 = SURFACE_STYLE_FILL_AREA ( #4840 ) ;
#2321 = VERTEX_POINT ( 'NONE', #1211 ) ;
#2322 = DIRECTION ( 'NONE',  ( -0.000000000000000000, 0.000000000000000000, 1.000000000000000000 ) ) ;
#2323 = LINE ( 'NONE', #5260, #14851 ) ;
#2324 = CARTESIAN_POINT ( 'NONE',  ( -15.19004016089065701, 13.79141621452552258, 96.37893023295546868 ) ) ;
#2325 = CARTESIAN_POINT ( 'NONE',  ( -15.53071739328007794, 28.07196708982276334, 102.0000000000000142 ) ) ;
#2326 = CARTESIAN_POINT ( 'NONE',  ( 50.00000000000000000, 26.78125000068279959, -6.123233995736766085E-15 ) ) ;
#2327 = CARTESIAN_POINT ( 'NONE',  ( 5.143516556418884111E-15, 52.00000000000000711, 42.00000000000000711 ) ) ;
#2328 = CARTESIAN_POINT ( 'NONE',  ( -5.000000000000000000, 90.58578643762692195, -1.414213562373097588 ) ) ;
#2329 = VECTOR ( 'NONE', #1220, 999.9999999999998863 ) ;
#2330 = CARTESIAN_POINT ( 'NONE',  ( -1.240322475938754499E-13, 36.28125000068280315, 50.00000000000000000 ) ) ;
#2331 = EDGE_CURVE ( 'NONE', #10856, #10814, #2549, .T. ) ;
#2332 = CARTESIAN_POINT ( 'NONE',  ( 7.919222016226807881, 49.44874571845315359, -50.00000000000000000 ) ) ;
#2333 = CARTESIAN_POINT ( 'NONE',  ( 50.00000000000000000, 48.78125000068279604, -6.123233995736766085E-15 ) ) ;
#2334 =( BOUNDED_CURVE ( )  B_SPLINE_CURVE ( 2, ( #14307, #11815, #6926, #501, #2755, #10415, #14220, #1514, #9164, #4092, #2845, #11980, #14457 ),
 .UNSPECIFIED., .F., .T. ) 
 B_SPLINE_CURVE_WITH_KNOTS ( ( 3, 2, 2, 2, 2, 2, 3 ),
 ( 0.6500000000000000222, 0.6533333333333333215, 0.6600000000000000311, 0.6666666666666666297, 0.6733333333333333393, 0.6800000000000000488, 0.6833333333333333481 ),
 .UNSPECIFIED. ) 
 CURVE ( )  GEOMETRIC_REPRESENTATION_ITEM ( )  RATIONAL_B_SPLINE_CURVE ( ( 0.9755282581475768211, 0.9755282581475771542, 1.000000000000000000, 0.9510565162951535312, 1.000000000000000000, 0.9510565162951535312, 1.000000000000000000, 0.9510565162951535312, 1.000000000000000000, 0.9510565162951535312, 1.000000000000000000, 0.9755282581475768211, 0.9755282581475768211 ) ) 
 REPRESENTATION_ITEM ( '' )  );
#2335 = CARTESIAN_POINT ( 'NONE',  ( 30.27664397204019409, 25.00000000000000355, -26.14048258526078072 ) ) ;
#2336 = CARTESIAN_POINT ( 'NONE',  ( 15.45084971874737789, 26.60000000000000142, 47.55282581475767500 ) ) ;
#2337 = CARTESIAN_POINT ( 'NONE',  ( -49.86468353124999453, 19.95937500034138878, 16.20201782572377525 ) ) ;
#2338 = CARTESIAN_POINT ( 'NONE',  ( -14.03285685708567065, 13.82077604687239258, 102.0000000000000142 ) ) ;
#2339 = CARTESIAN_POINT ( 'NONE',  ( -49.86468353125000164, 43.85937500034140157, 0.000000000000000000 ) ) ;
#2340 = EDGE_LOOP ( 'NONE', ( #12527, #12705 ) ) ;
#2341 = CARTESIAN_POINT ( 'NONE',  ( -49.86468353124999453, 25.75937500034139660, -16.20201782572375393 ) ) ;
#2342 = ORIENTED_EDGE ( 'NONE', *, *, #15755, .T. ) ;
#2343 = CARTESIAN_POINT ( 'NONE',  ( 50.00000000000000000, 49.00000000000000000, -6.123233995736766085E-15 ) ) ;
#2344 = CARTESIAN_POINT ( 'NONE',  ( 30.81806926056964002, 38.55937500034140442, 42.41743335407647209 ) ) ;
#2345 = EDGE_CURVE ( 'NONE', #2458, #11124, #10403, .T. ) ;
#2346 = CARTESIAN_POINT ( 'NONE',  ( 1.293669679204937499E-13, 41.28125000068279604, -50.00000000000000000 ) ) ;
#2347 = CARTESIAN_POINT ( 'NONE',  ( 13.22516817658054933, 40.70288237343638826, 101.0000000000000000 ) ) ;
#2348 = CARTESIAN_POINT ( 'NONE',  ( 46.25745152662987891, 25.00000000000000000, -18.62156331807923593 ) ) ;
#2349 = EDGE_CURVE ( 'NONE', #11917, #15953, #722, .T. ) ;
#2350 = CARTESIAN_POINT ( 'NONE',  ( -40.34137639590981195, 20.12187500034139731, 29.30972558990012189 ) ) ;
#2351 = CARTESIAN_POINT ( 'NONE',  ( -49.86468353125000164, 31.85937500034139447, 0.000000000000000000 ) ) ;
#2352 = PLANE ( 'NONE',  #5274 ) ;
#2353 = CARTESIAN_POINT ( 'NONE',  ( 9.631387414534489405E-15, 36.42187500034139447, 52.43083105670540789 ) ) ;
#2354 = LINE ( 'NONE', #12578, #693 ) ;
#2355 = CARTESIAN_POINT ( 'NONE',  ( 9.657523855033129090E-15, 36.50000000000000711, 52.57311121191334990 ) ) ;
#2356 = CARTESIAN_POINT ( 'NONE',  ( -49.86468353124999453, 39.95937500034139589, 16.20201782572377525 ) ) ;
#2357 = CARTESIAN_POINT ( 'NONE',  ( 9.631387414534489405E-15, 36.42187500034139447, 52.43083105670540789 ) ) ;
#2358 = EDGE_CURVE ( 'NONE', #15408, #2396, #13233, .T. ) ;
#2359 = CARTESIAN_POINT ( 'NONE',  ( -15.45084971874736368, 44.39999999999999858, 47.55282581475768211 ) ) ;
#2360 = ORIENTED_EDGE ( 'NONE', *, *, #1971, .F. ) ;
#2361 = CARTESIAN_POINT ( 'NONE',  ( 40.34137639590981195, 45.05937500034139731, -29.30972558990011834 ) ) ;
#2362 = EDGE_LOOP ( 'NONE', ( #6480, #9687, #1391, #13902 ) ) ;
#2363 = CARTESIAN_POINT ( 'NONE',  ( -15.45084971874737256, 21.38125000068279746, -47.55282581475767500 ) ) ;
#2364 = AXIS2_PLACEMENT_3D ( 'NONE', #1989, #7085, #991 ) ;
#2365 = CARTESIAN_POINT ( 'NONE',  ( 0.000000000000000000, 0.000000000000000000, 0.000000000000000000 ) ) ;
#2366 = FACE_OUTER_BOUND ( 'NONE', #5595, .T. ) ;
#2367 = CARTESIAN_POINT ( 'NONE',  ( -15.40903463028481646, 39.52187500034139589, -47.42413220539093999 ) ) ;
#2368 = CARTESIAN_POINT ( 'NONE',  ( 1.293669679204937499E-13, 41.50000000000000000, -50.00000000000000000 ) ) ;
#2369 = CARTESIAN_POINT ( 'NONE',  ( -15.40903463028480580, 26.32187500034140015, 47.42413220539094709 ) ) ;
#2370 = CARTESIAN_POINT ( 'NONE',  ( 50.00000000000000000, 24.78125000068279959, -6.123233995736766085E-15 ) ) ;
#2371 = EDGE_CURVE ( 'NONE', #13515, #8474, #11913, .T. ) ;
#2372 = CARTESIAN_POINT ( 'NONE',  ( 15.40903463028482356, 34.52187500034140299, 47.42413220539093999 ) ) ;
#2373 = CARTESIAN_POINT ( 'NONE',  ( -25.03223043950028881, 286.3455096218659151, -2.564460878999442084 ) ) ;
#2374 = CARTESIAN_POINT ( 'NONE',  ( 15.40903463028482356, 34.52187500034140299, 47.42413220539093999 ) ) ;
#2375 = DIRECTION ( 'NONE',  ( -0.000000000000000000, -0.000000000000000000, 1.000000000000000000 ) ) ;
#2376 = ORIENTED_EDGE ( 'NONE', *, *, #1542, .F. ) ;
#2377 = ORIENTED_EDGE ( 'NONE', *, *, #14727, .T. ) ;
#2378 = EDGE_LOOP ( 'NONE', ( #11285, #1066, #14759, #8367 ) ) ;
#2379 = CARTESIAN_POINT ( 'NONE',  ( -15.45084971874737256, 31.60000000000000142, -47.55282581475767500 ) ) ;
#2380 = FACE_OUTER_BOUND ( 'NONE', #2438, .T. ) ;
#2381 = CARTESIAN_POINT ( 'NONE',  ( -7.919222016226934890, 22.22999571913594963, 49.99999999999996447 ) ) ;
#2382 = CARTESIAN_POINT ( 'NONE',  ( 9.189545401991395579, 24.96013318841451678, 102.0000000000000142 ) ) ;
#2383 = CARTESIAN_POINT ( 'NONE',  ( 49.86468353124999453, 32.95937500034138168, -16.20201782572376459 ) ) ;
#2384 = CARTESIAN_POINT ( 'NONE',  ( 9.227956911499398113E-15, 102.0000000000000142, -1.913737646857611713E-14 ) ) ;
#2385 = DIRECTION ( 'NONE',  ( 0.000000000000000000, 1.000000000000000000, 0.000000000000000000 ) ) ;
#2386 =( LENGTH_UNIT ( ) NAMED_UNIT ( * ) SI_UNIT ( .MILLI., .METRE. ) );
#2387 = CARTESIAN_POINT ( 'NONE',  ( 0.000000000000000000, 272.0000000000000000, 0.000000000000000000 ) ) ;
#2388 = CYLINDRICAL_SURFACE ( 'NONE', #6073, 50.00000000000000000 ) ;
#2389 = CARTESIAN_POINT ( 'NONE',  ( 15.45084971874736723, 25.18125000068279817, -47.55282581475768211 ) ) ;
#2390 = EDGE_LOOP ( 'NONE', ( #1940, #14090 ) ) ;
#2391 = EDGE_CURVE ( 'NONE', #3858, #9016, #6881, .T. ) ;
#2392 = CARTESIAN_POINT ( 'NONE',  ( 49.86468353124999453, 24.95937500034139234, -16.20201782572376459 ) ) ;
#2393 =( BOUNDED_CURVE ( )  B_SPLINE_CURVE ( 3, ( #6008, #10830, #9582, #7252 ),
 .UNSPECIFIED., .F., .F. ) 
 B_SPLINE_CURVE_WITH_KNOTS ( ( 4, 4 ),
 ( 4.523772594209285458, 4.712388980384689674 ),
 .UNSPECIFIED. ) 
 CURVE ( )  GEOMETRIC_REPRESENTATION_ITEM ( )  RATIONAL_B_SPLINE_CURVE ( ( 1.000000000000000000, 0.9970375182503885547, 0.9970375182503885547, 1.000000000000000000 ) ) 
 REPRESENTATION_ITEM ( '' )  );
#2394 = EDGE_CURVE ( 'NONE', #12657, #2563, #15354, .T. ) ;
#2395 = ORIENTED_EDGE ( 'NONE', *, *, #10165, .T. ) ;
#2396 = VERTEX_POINT ( 'NONE', #12147 ) ;
#2397 = EDGE_LOOP ( 'NONE', ( #16288, #625, #15296, #11611 ) ) ;
#2398 = CARTESIAN_POINT ( 'NONE',  ( 30.90169943749474157, 39.08125000068280031, -42.53254041760200721 ) ) ;
#2399 = CARTESIAN_POINT ( 'NONE',  ( 7.919222016226809657, 35.22999571913594963, -50.00000000000000000 ) ) ;
#2400 = CARTESIAN_POINT ( 'NONE',  ( -8.660254037844415720, 37.00000000000001421, -4.999999999999952038 ) ) ;
#2401 = ORIENTED_EDGE ( 'NONE', *, *, #794, .T. ) ;
#2402 = PLANE ( 'NONE',  #7030 ) ;
#2403 = DIRECTION ( 'NONE',  ( -0.000000000000000000, 1.000000000000000000, -0.000000000000000000 ) ) ;
#2404 = CARTESIAN_POINT ( 'NONE',  ( -7.827029700262156275, 6.837221630493822921, 98.48522124286309065 ) ) ;
#2405 = DIRECTION ( 'NONE',  ( -0.000000000000000000, -1.000000000000000000, -0.000000000000000000 ) ) ;
#2406 = CARTESIAN_POINT ( 'NONE',  ( 15.45084971874736723, 27.18125000068279817, -47.55282581475768211 ) ) ;
#2407 = DIRECTION ( 'NONE',  ( 5.069245582283711292E-17, 1.000000000000000000, -8.780190904559503697E-17 ) ) ;
#2408 = CARTESIAN_POINT ( 'NONE',  ( -43.87482193696061472, 262.0000000000000000, 10.00000000000000178 ) ) ;
#2409 = LINE ( 'NONE', #16464, #4097 ) ;
#2410 = CARTESIAN_POINT ( 'NONE',  ( 9.657523855033129090E-15, 48.28125000068279604, 52.57311121191334990 ) ) ;
#2411 = CARTESIAN_POINT ( 'NONE',  ( 6.251299836021209089, 37.76994598419266680, 102.0000000000000142 ) ) ;
#2412 = CARTESIAN_POINT ( 'NONE',  ( -40.45084971874737789, 23.80000000000000071, -29.38926261462365730 ) ) ;
#2413 = LINE ( 'NONE', #11322, #3894 ) ;
#2414 = CARTESIAN_POINT ( 'NONE',  ( 7.513064459987437071E-14, 42.28125000068280315, 50.00000000000000000 ) ) ;
#2415 = CARTESIAN_POINT ( 'NONE',  ( -30.81806926056962226, 42.15937500034139163, 42.41743335407647919 ) ) ;
#2416 = ORIENTED_EDGE ( 'NONE', *, *, #15170, .F. ) ;
#2417 = ORIENTED_EDGE ( 'NONE', *, *, #13348, .F. ) ;
#2418 = B_SPLINE_CURVE_WITH_KNOTS ( 'NONE', 3,
 ( #11442, #4120, #10281, #9029, #14084, #14166, #6631, #1287, #114, #12601, #280, #6294, #7776, #15418, #12847, #1367, #7698, #2700, #9107, #9192, #7528, #3874, #1450, #6378, #6542, #2450 ),
 .UNSPECIFIED., .F., .F.,
 ( 4, 2, 2, 2, 2, 2, 2, 2, 2, 2, 2, 2, 4 ),
 ( 0.04214985370082251215, 0.04558239031788638429, 0.04729865862641832036, 0.04901492693495026337, 0.05244746355201414245, 0.05416373186054608546, 0.05588000016907802847, 0.05759626847760997148, 0.05931253678614191449, 0.06274507340320578663, 0.06446134171173772964, 0.06617761002026967265, 0.06961014663733354479 ),
 .UNSPECIFIED. ) ;
#2419 = DIRECTION ( 'NONE',  ( 2.312964634635742464E-16, -0.000000000000000000, 1.000000000000000000 ) ) ;
#2420 = CARTESIAN_POINT ( 'NONE',  ( -15.40903463028480580, 28.25937500034139660, 47.42413220539094709 ) ) ;
#2421 = CARTESIAN_POINT ( 'NONE',  ( 0.000000000000000000, 54.00000000000000711, 0.000000000000000000 ) ) ;
#2422 = LINE ( 'NONE', #13734, #11051 ) ;
#2423 = CARTESIAN_POINT ( 'NONE',  ( 45.67643563158024023, 25.00000000000000000, -20.00444126042648207 ) ) ;
#2424 =( BOUNDED_CURVE ( )  B_SPLINE_CURVE ( 3, ( #9395, #10571, #4328, #13054 ),
 .UNSPECIFIED., .F., .T. ) 
 B_SPLINE_CURVE_WITH_KNOTS ( ( 4, 4 ),
 ( 4.712388980384689674, 4.901005366560093890 ),
 .UNSPECIFIED. ) 
 CURVE ( )  GEOMETRIC_REPRESENTATION_ITEM ( )  RATIONAL_B_SPLINE_CURVE ( ( 1.000000000000000000, 0.9970375182503885547, 0.9970375182503885547, 1.000000000000000000 ) ) 
 REPRESENTATION_ITEM ( '' )  );
#2425 = CARTESIAN_POINT ( 'NONE',  ( 49.99999999999999289, 30.88125000068279746, -16.24598481164532160 ) ) ;
#2426 = CARTESIAN_POINT ( 'NONE',  ( -49.86468353124999453, 23.82187500034139305, -16.20201782572375393 ) ) ;
#2427 = CARTESIAN_POINT ( 'NONE',  ( -49.86468353124999453, 23.75937500034139660, -16.20201782572375393 ) ) ;
#2428 = CARTESIAN_POINT ( 'NONE',  ( 50.00000000000000000, 43.00000000000000000, -6.123233995736766085E-15 ) ) ;
#2429 = CARTESIAN_POINT ( 'NONE',  ( -15.40903463028481646, 37.52187500034139589, -47.42413220539093999 ) ) ;
#2430 = DIRECTION ( 'NONE',  ( -0.000000000000000000, 1.000000000000000000, -0.000000000000000000 ) ) ;
#2431 = CARTESIAN_POINT ( 'NONE',  ( 30.90169943749474157, 35.30000000000000426, -42.53254041760200721 ) ) ;
#2432 = CARTESIAN_POINT ( 'NONE',  ( -3.210462471511496205E-15, 39.35937500034138736, -52.43083105670540789 ) ) ;
#2433 = CARTESIAN_POINT ( 'NONE',  ( -49.86468353124999453, 33.82187500034138594, -16.20201782572375393 ) ) ;
#2434 = ADVANCED_FACE ( 'NONE', ( #7168 ), #10980, .F. ) ;
#2435 = CARTESIAN_POINT ( 'NONE',  ( -15.45084971874737256, 43.60000000000000142, -47.55282581475767500 ) ) ;
#2436 = ORIENTED_EDGE ( 'NONE', *, *, #5698, .F. ) ;
#2437 = CARTESIAN_POINT ( 'NONE',  ( 40.34137639590981195, 35.05937500034139731, -29.30972558990011834 ) ) ;
#2438 = EDGE_LOOP ( 'NONE', ( #1392, #10459, #15571, #7122 ) ) ;
#2439 = EDGE_LOOP ( 'NONE', ( #6445, #15228, #12358, #5102, #1525 ) ) ;
#2441 = EDGE_CURVE ( 'NONE', #12025, #9639, #13383, .T. ) ;
#2440 = CARTESIAN_POINT ( 'NONE',  ( -3.219174618344376363E-15, 23.28125000068279959, -52.57311121191334990 ) ) ;
#2442 = CARTESIAN_POINT ( 'NONE',  ( -50.00000000000000000, 34.00000000000000000, 0.000000000000000000 ) ) ;
#2443 = CARTESIAN_POINT ( 'NONE',  ( -3.210462471511496205E-15, 23.42187500034139802, -52.43083105670540789 ) ) ;
#2444 = CARTESIAN_POINT ( 'NONE',  ( -27.07106781186547551, 282.0000000000000000, 6.642135623730951899 ) ) ;
#2445 = EDGE_CURVE ( 'NONE', #1138, #5870, #13520, .T. ) ;
#2446 = CARTESIAN_POINT ( 'NONE',  ( -30.81806926056962226, 40.22187500034139873, 42.41743335407647919 ) ) ;
#2447 = DIRECTION ( 'NONE',  ( 0.000000000000000000, -1.000000000000000000, 0.000000000000000000 ) ) ;
#2448 = CARTESIAN_POINT ( 'NONE',  ( 40.45084971874737789, 48.80000000000000426, 29.38926261462365375 ) ) ;
#2449 = CARTESIAN_POINT ( 'NONE',  ( 50.00000000000000711, 26.68125000068279462, 16.24598481164530739 ) ) ;
#2450 = CARTESIAN_POINT ( 'NONE',  ( -2.317185599438165467E-15, 40.00000000000004974, 92.94692077166139654 ) ) ;
#2451 = EDGE_CURVE ( 'NONE', #9157, #2703, #4847, .T. ) ;
#2452 = CARTESIAN_POINT ( 'NONE',  ( -49.86468353124999453, 31.82187500034139305, -16.20201782572375393 ) ) ;
#2453 = CARTESIAN_POINT ( 'NONE',  ( -25.07567824489025199, 285.0109613520617131, -7.575678244888824686 ) ) ;
#2454 = CARTESIAN_POINT ( 'NONE',  ( -40.34137639590981905, 33.72187500034139873, -29.30972558990011478 ) ) ;
#2455 = CARTESIAN_POINT ( 'NONE',  ( -7.919222016226773242, 42.22999571913594963, 50.00000000000000711 ) ) ;
#2456 = ORIENTED_EDGE ( 'NONE', *, *, #14582, .T. ) ;
#2457 = AXIS2_PLACEMENT_3D ( 'NONE', #1972, #13216, #3068 ) ;
#2458 = VERTEX_POINT ( 'NONE', #12480 ) ;
#2459 = FACE_OUTER_BOUND ( 'NONE', #4151, .T. ) ;
#2460 = DIRECTION ( 'NONE',  ( 0.000000000000000000, 0.000000000000000000, 1.000000000000000000 ) ) ;
#2461 = CARTESIAN_POINT ( 'NONE',  ( -15.45084971874736368, 24.40000000000000213, 47.55282581475768211 ) ) ;
#2462 = CARTESIAN_POINT ( 'NONE',  ( -25.00000000000000355, 287.0000000000000568, 7.500000000000001776 ) ) ;
#2463 = CARTESIAN_POINT ( 'NONE',  ( 40.34137639590981195, 29.05937500034139376, -29.30972558990011834 ) ) ;
#2464 = SURFACE_STYLE_FILL_AREA ( #8872 ) ;
#2465 = CARTESIAN_POINT ( 'NONE',  ( -30.81806926056963292, 47.62187500034139731, -42.41743335407646498 ) ) ;
#2466 = FILL_AREA_STYLE_COLOUR ( '', #10529 ) ;
#2467 = CARTESIAN_POINT ( 'NONE',  ( -7.571758127758879908, 38.27715053026740577, 101.0000000000000000 ) ) ;
#2468 = EDGE_CURVE ( 'NONE', #7372, #2224, #3246, .T. ) ;
#2469 = VECTOR ( 'NONE', #6768, 1000.000000000000000 ) ;
#2470 = FACE_OUTER_BOUND ( 'NONE', #5821, .T. ) ;
#2471 = DIRECTION ( 'NONE',  ( 1.000000000000000000, 0.000000000000000000, 0.000000000000000000 ) ) ;
#2472 = ORIENTED_EDGE ( 'NONE', *, *, #5004, .T. ) ;
#2473 = B_SPLINE_CURVE_WITH_KNOTS ( 'NONE', 3,
 ( #1469, #5396, #10455, #15512 ),
 .UNSPECIFIED., .F., .F.,
 ( 4, 4 ),
 ( 0.000000000000000000, 0.01231015999390750251 ),
 .UNSPECIFIED. ) ;
#2474 = CARTESIAN_POINT ( 'NONE',  ( 30.81806926056962936, 23.15937500034139873, -42.41743335407647209 ) ) ;
#2475 = ORIENTED_EDGE ( 'NONE', *, *, #8085, .T. ) ;
#2476 = VERTEX_POINT ( 'NONE', #15965 ) ;
#2477 = EDGE_LOOP ( 'NONE', ( #3235, #12674, #6153, #11970 ) ) ;
#2478 = ORIENTED_EDGE ( 'NONE', *, *, #3150, .T. ) ;
#2479 = CYLINDRICAL_SURFACE ( 'NONE', #3382, 79.49773270518484480 ) ;
#2480 = CARTESIAN_POINT ( 'NONE',  ( 4.898587196589413026E-15, 217.0000000000000284, -40.00000000000000000 ) ) ;
#2481 = VECTOR ( 'NONE', #13307, 1000.000000000000000 ) ;
#2482 = CARTESIAN_POINT ( 'NONE',  ( 8.446640517145639571E-15, 28.49999999999999645, 50.00000000000000000 ) ) ;
#2483 = FACE_OUTER_BOUND ( 'NONE', #12356, .T. ) ;
#2484 = CARTESIAN_POINT ( 'NONE',  ( -30.81806926056963292, 49.55937500034139731, -42.41743335407647209 ) ) ;
#2485 = DIRECTION ( 'NONE',  ( 1.000000000000000000, 0.000000000000000000, 0.000000000000000000 ) ) ;
#2486 = CARTESIAN_POINT ( 'NONE',  ( 3.505380114644276013, 97.73782665365222044, -8.566253778398381868 ) ) ;
#2487 = CARTESIAN_POINT ( 'NONE',  ( 7.919222016226809657, 25.22999571913595318, -50.00000000000000000 ) ) ;
#2488 = FACE_OUTER_BOUND ( 'NONE', #20, .T. ) ;
#2489 = ADVANCED_FACE ( 'NONE', ( #6091 ), #8318, .F. ) ;
#2490 = APPLICATION_CONTEXT ( 'automotive_design' ) ;
#2491 = CARTESIAN_POINT ( 'NONE',  ( -15.45084971874736368, 48.18125000068280173, 47.55282581475768211 ) ) ;
#2492 = DIRECTION ( 'NONE',  ( 0.2079116908177664202, -0.9781476007338041345, 0.000000000000000000 ) ) ;
#2493 = CARTESIAN_POINT ( 'NONE',  ( 50.00000000000000000, 23.00000000000000355, -6.123233995736766085E-15 ) ) ;
#2494 = CARTESIAN_POINT ( 'NONE',  ( -30.81806926056963292, 21.55937500034140086, -42.41743335407647209 ) ) ;
#2495 = CARTESIAN_POINT ( 'NONE',  ( -3.111920190527341144E-15, 29.50000000000000000, -50.00000000000000000 ) ) ;
#2496 = CARTESIAN_POINT ( 'NONE',  ( 40.34137639590981905, 42.65937500034139873, 29.30972558990010768 ) ) ;
#2497 = ORIENTED_EDGE ( 'NONE', *, *, #7202, .T. ) ;
#2498 = EDGE_LOOP ( 'NONE', ( #5485, #3317, #14275, #955, #738, #6323, #1719 ) ) ;
#2499 = LINE ( 'NONE', #10238, #8412 ) ;
#2500 = CARTESIAN_POINT ( 'NONE',  ( 49.86468353125001585, 28.75937500034139305, 16.20201782572375038 ) ) ;
#2501 = CARTESIAN_POINT ( 'NONE',  ( 15.45084971874736723, 33.39999999999999858, -47.55282581475768211 ) ) ;
#2502 = CARTESIAN_POINT ( 'NONE',  ( -14.89227969048185152, 31.70859663795358330, 93.22745684670599076 ) ) ;
#2503 = CARTESIAN_POINT ( 'NONE',  ( 48.07045810499300842, 25.00000000000000000, -13.25585611146359177 ) ) ;
#2504 = CARTESIAN_POINT ( 'NONE',  ( -30.81806926056962226, 32.22187500034139163, 42.41743335407647209 ) ) ;
#2505 = AXIS2_PLACEMENT_3D ( 'NONE', #14076, #2691, #3785 ) ;
#2506 = LINE ( 'NONE', #11570, #11062 ) ;
#2507 = CARTESIAN_POINT ( 'NONE',  ( -40.34137639590981195, 22.12187500034139731, 29.30972558990012189 ) ) ;
#2508 = CARTESIAN_POINT ( 'NONE',  ( -15.40903463028480580, 20.25937500034139660, 47.42413220539094709 ) ) ;
#2509 = CARTESIAN_POINT ( 'NONE',  ( 40.45084971874737079, 43.20000000000000284, -29.38926261462366440 ) ) ;
#2510 = CARTESIAN_POINT ( 'NONE',  ( -15.40903463028480580, 38.32187500034140015, 47.42413220539094709 ) ) ;
#2511 = DIRECTION ( 'NONE',  ( 0.000000000000000000, 0.000000000000000000, 1.000000000000000000 ) ) ;
#2512 = CARTESIAN_POINT ( 'NONE',  ( -50.00000000000000000, 34.00000000000000000, 0.000000000000000000 ) ) ;
#2513 = CARTESIAN_POINT ( 'NONE',  ( 15.40903463028481113, 37.25937500034140015, -47.42413220539094709 ) ) ;
#2514 = CARTESIAN_POINT ( 'NONE',  ( -30.81806926056962226, 32.22187500034139163, 42.41743335407647919 ) ) ;
#2515 = CARTESIAN_POINT ( 'NONE',  ( -30.90169943749473802, 42.30000000000000426, 42.53254041760200721 ) ) ;
#2516 = VERTEX_POINT ( 'NONE', #13471 ) ;
#2517 = VECTOR ( 'NONE', #616, 1000.000000000000114 ) ;
#2518 = EDGE_LOOP ( 'NONE', ( #1350, #9486, #15705, #9836 ) ) ;
#2520 = EDGE_CURVE ( 'NONE', #1226, #4102, #6891, .T. ) ;
#2519 = VECTOR ( 'NONE', #16394, 1000.000000000000000 ) ;
#2521 = CARTESIAN_POINT ( 'NONE',  ( -3.210462471511496205E-15, 39.35937500034138736, -52.43083105670540789 ) ) ;
#2522 = ADVANCED_FACE ( 'NONE', ( #16044 ), #9539, .T. ) ;
#2523 = EDGE_LOOP ( 'NONE', ( #15213, #12449 ) ) ;
#2524 = VERTEX_POINT ( 'NONE', #2327 ) ;
#2525 = CARTESIAN_POINT ( 'NONE',  ( 0.000000000000000000, 262.0000000000000000, 0.000000000000000000 ) ) ;
#2527 =( BOUNDED_CURVE ( )  B_SPLINE_CURVE ( 2, ( #11646, #1578, #638, #3486, #12211, #8301, #7151, #10809, #10961, #13837, #3227, #10719, #13535 ),
 .UNSPECIFIED., .F., .T. ) 
 B_SPLINE_CURVE_WITH_KNOTS ( ( 3, 2, 2, 2, 2, 2, 3 ),
 ( 0.1166666666666666685, 0.1199999999999999956, 0.1266666666666666774, 0.1333333333333333315, 0.1400000000000000133, 0.1466666666666666674, 0.1499999999999999944 ),
 .UNSPECIFIED. ) 
 CURVE ( )  GEOMETRIC_REPRESENTATION_ITEM ( )  RATIONAL_B_SPLINE_CURVE ( ( 0.9755282581475768211, 0.9755282581475768211, 1.000000000000000000, 0.9510565162951535312, 1.000000000000000000, 0.9510565162951535312, 1.000000000000000000, 0.9510565162951535312, 1.000000000000000000, 0.9510565162951535312, 1.000000000000000000, 0.9755282581475768211, 0.9755282581475768211 ) ) 
 REPRESENTATION_ITEM ( '' )  );
#2526 = CARTESIAN_POINT ( 'NONE',  ( -15.40903463028481646, 49.45937500034140299, -47.42413220539093999 ) ) ;
#2528 = PLANE ( 'NONE',  #6500 ) ;
#2529 = CARTESIAN_POINT ( 'NONE',  ( 9.631387414534489405E-15, 26.42187500034139447, 52.43083105670540789 ) ) ;
#2530 = DIRECTION ( 'NONE',  ( 0.000000000000000000, 0.000000000000000000, 1.000000000000000000 ) ) ;
#2531 = CARTESIAN_POINT ( 'NONE',  ( 30.81806926056962936, 41.22187500034139873, -42.41743335407647209 ) ) ;
#2532 = VECTOR ( 'NONE', #14359, 1000.000000000000000 ) ;
#2533 = CARTESIAN_POINT ( 'NONE',  ( -49.99999999999999289, 48.10000000000000142, 16.24598481164533226 ) ) ;
#2534 = CARTESIAN_POINT ( 'NONE',  ( -15.45084971874736368, 28.18125000068279817, 47.55282581475768211 ) ) ;
#2535 = ADVANCED_FACE ( 'NONE', ( #14791, #8485 ), #5836, .T. ) ;
#2536 = CARTESIAN_POINT ( 'NONE',  ( -30.81806926056963292, 47.62187500034139731, -42.41743335407647209 ) ) ;
#2537 = CARTESIAN_POINT ( 'NONE',  ( 15.40903463028481113, 35.32187500034139305, -47.42413220539094709 ) ) ;
#2538 = CARTESIAN_POINT ( 'NONE',  ( -2.445080149700054274E-14, 46.50000000000000711, 50.00000000000000000 ) ) ;
#2539 = CARTESIAN_POINT ( 'NONE',  ( 3.505380114644273348, 100.5662537783983765, 8.566253778398346341 ) ) ;
#2540 = ORIENTED_EDGE ( 'NONE', *, *, #9370, .F. ) ;
#2541 = CIRCLE ( 'NONE', #5733, 40.00000000000000000 ) ;
#2542 = AXIS2_PLACEMENT_3D ( 'NONE', #15257, #6388, #7868 ) ;
#2543 = VECTOR ( 'NONE', #8638, 1000.000000000000227 ) ;
#2544 = VERTEX_POINT ( 'NONE', #13551 ) ;
#2545 = CARTESIAN_POINT ( 'NONE',  ( -40.45084971874737079, 32.20000000000000284, 29.38926261462367151 ) ) ;
#2546 = LINE ( 'NONE', #2297, #2253 ) ;
#2547 = ADVANCED_FACE ( 'NONE', ( #2156 ), #7245, .T. ) ;
#2548 = CARTESIAN_POINT ( 'NONE',  ( -7.977241335952133916, 17.31698729810774751, 101.0000000000000000 ) ) ;
#2549 = LINE ( 'NONE', #6306, #10050 ) ;
#2550 = CARTESIAN_POINT ( 'NONE',  ( 49.86468353125001585, 28.75937500034139305, 16.20201782572375038 ) ) ;
#2551 = CARTESIAN_POINT ( 'NONE',  ( -49.86468353125000164, 45.92187500034139447, 0.000000000000000000 ) ) ;
#2552 = PRESENTATION_STYLE_ASSIGNMENT (( #14019 ) ) ;
#2553 = CIRCLE ( 'NONE', #13434, 17.50000000000000000 ) ;
#2555 = CARTESIAN_POINT ( 'NONE',  ( -30.90169943749474513, 39.69999999999999574, -42.53254041760200721 ) ) ;
#2554 = AXIS2_PLACEMENT_3D ( 'NONE', #15387, #4009, #9079 ) ;
#2556 = AXIS2_PLACEMENT_3D ( 'NONE', #1237, #3744, #6331 ) ;
#2557 = ADVANCED_FACE ( 'NONE', ( #11071 ), #4767, .T. ) ;
#2558 = DIRECTION ( 'NONE',  ( -0.5877852522924797984, 0.8090169943749424553, 0.000000000000000000 ) ) ;
#2559 = LINE ( 'NONE', #51, #3258 ) ;
#2560 = ORIENTED_EDGE ( 'NONE', *, *, #12839, .T. ) ;
#2561 = ADVANCED_FACE ( 'NONE', ( #8981 ), #11314, .F. ) ;
#2562 = CARTESIAN_POINT ( 'NONE',  ( 49.86468353125000164, 22.85937500034139802, -6.106662507704105588E-15 ) ) ;
#2563 = VERTEX_POINT ( 'NONE', #8728 ) ;
#2564 = LINE ( 'NONE', #7643, #8117 ) ;
#2565 = ORIENTED_EDGE ( 'NONE', *, *, #99, .T. ) ;
#2566 = ORIENTED_EDGE ( 'NONE', *, *, #5224, .T. ) ;
#2567 = AXIS2_PLACEMENT_3D ( 'NONE', #8509, #15911, #13493 ) ;
#2568 = DIRECTION ( 'NONE',  ( 0.000000000000000000, -0.000000000000000000, -1.000000000000000000 ) ) ;
#2569 = CARTESIAN_POINT ( 'NONE',  ( 0.000000000000000000, 193.4213562373095385, -50.00000000000000000 ) ) ;
#2570 = AXIS2_PLACEMENT_3D ( 'NONE', #4839, #4664, #13620 ) ;
#2571 =( LENGTH_UNIT ( ) NAMED_UNIT ( * ) SI_UNIT ( .MILLI., .METRE. ) );
#2572 = CARTESIAN_POINT ( 'NONE',  ( 0.000000000000000000, 22.50000000000000000, 101.0000000000000000 ) ) ;
#2573 = DIRECTION ( 'NONE',  ( -1.000000000000000000, 0.000000000000000000, 0.000000000000000000 ) ) ;
#2574 = CARTESIAN_POINT ( 'NONE',  ( -43.87482193696061472, 257.0000000000001137, -10.00000000000000178 ) ) ;
#2575 = DIRECTION ( 'NONE',  ( -0.000000000000000000, -1.000000000000000000, -0.000000000000000000 ) ) ;
#2576 = CARTESIAN_POINT ( 'NONE',  ( 40.45084971874737079, 24.98125000068279888, -29.38926261462366440 ) ) ;
#2577 =( BOUNDED_CURVE ( )  B_SPLINE_CURVE ( 3, ( #8071, #11978, #5598, #8162 ),
 .UNSPECIFIED., .F., .F. ) 
 B_SPLINE_CURVE_WITH_KNOTS ( ( 4, 4 ),
 ( 4.712388980384689674, 6.283185307179586232 ),
 .UNSPECIFIED. ) 
 CURVE ( )  GEOMETRIC_REPRESENTATION_ITEM ( )  RATIONAL_B_SPLINE_CURVE ( ( 1.000000000000000000, 0.8047378541243649375, 0.8047378541243649375, 1.000000000000000000 ) ) 
 REPRESENTATION_ITEM ( '' )  );
#2578 = CARTESIAN_POINT ( 'NONE',  ( -50.00000000000000000, 50.00000000000000000, 0.000000000000000000 ) ) ;
#2579 = CARTESIAN_POINT ( 'NONE',  ( 40.45084971874737789, 40.58125000068280031, 29.38926261462365375 ) ) ;
#2580 = DIRECTION ( 'NONE',  ( 0.9781476007338041345, 0.2079116908177664202, 0.000000000000000000 ) ) ;
#2581 = AXIS2_PLACEMENT_3D ( 'NONE', #15699, #240, #10476 ) ;
#2582 = CARTESIAN_POINT ( 'NONE',  ( -3.219174618344376363E-15, 21.50000000000000355, -52.57311121191334990 ) ) ;
#2583 = DIRECTION ( 'NONE',  ( 0.000000000000000000, 0.000000000000000000, 1.000000000000000000 ) ) ;
#2584 = ADVANCED_FACE ( 'NONE', ( #3671 ), #6491, .T. ) ;
#2585 = ORIENTED_EDGE ( 'NONE', *, *, #16278, .T. ) ;
#2586 = VECTOR ( 'NONE', #7969, 1000.000000000000000 ) ;
#2587 = CARTESIAN_POINT ( 'NONE',  ( -40.34137639590981195, 44.05937500034139731, 29.30972558990012189 ) ) ;
#2588 = ORIENTED_EDGE ( 'NONE', *, *, #8894, .T. ) ;
#2589 = DIRECTION ( 'NONE',  ( 1.000000000000000000, 0.000000000000000000, 0.000000000000000000 ) ) ;
#2590 = LINE ( 'NONE', #12895, #1775 ) ;
#2591 = CARTESIAN_POINT ( 'NONE',  ( 49.86468353125000164, 28.85937500034139802, -6.106662507704105588E-15 ) ) ;
#2592 = ORIENTED_EDGE ( 'NONE', *, *, #1625, .F. ) ;
#2593 = CARTESIAN_POINT ( 'NONE',  ( 5.853156874688941503E-15, 82.00000000000001421, -24.08089297201393109 ) ) ;
#2594 = CARTESIAN_POINT ( 'NONE',  ( 45.25922935877483155, 25.00000000000000000, -20.93126818148093804 ) ) ;
#2595 = CARTESIAN_POINT ( 'NONE',  ( 40.34137639590981195, 33.12187500034139731, -29.30972558990011834 ) ) ;
#2596 = DIRECTION ( 'NONE',  ( -0.9945218953682744001, 0.1045284632676435205, 0.000000000000000000 ) ) ;
#2597 = CARTESIAN_POINT ( 'NONE',  ( 15.40903463028481113, 25.25937500034139660, -47.42413220539094709 ) ) ;
#2598 = EDGE_CURVE ( 'NONE', #8439, #16202, #5043, .T. ) ;
#2599 = CARTESIAN_POINT ( 'NONE',  ( 40.34137639590981195, 37.12187500034139731, -29.30972558990011834 ) ) ;
#2600 = DIRECTION ( 'NONE',  ( 0.000000000000000000, -1.000000000000000000, 0.000000000000000000 ) ) ;
#2601 = CARTESIAN_POINT ( 'NONE',  ( -40.45084971874737079, 30.20000000000000284, 29.38926261462367151 ) ) ;
#2602 = ADVANCED_FACE ( 'NONE', ( #5264 ), #7653, .T. ) ;
#2603 = CARTESIAN_POINT ( 'NONE',  ( 40.34137639590981195, 39.05937500034140442, -29.30972558990011834 ) ) ;
#2604 = CARTESIAN_POINT ( 'NONE',  ( -30.81806926056962226, 30.22187500034139518, 42.41743335407647919 ) ) ;
#2605 = CARTESIAN_POINT ( 'NONE',  ( -3.219174618344376363E-15, 43.50000000000000000, -52.57311121191334990 ) ) ;
#2606 = AXIS2_PLACEMENT_3D ( 'NONE', #5818, #131, #5078 ) ;
#2607 = ORIENTED_EDGE ( 'NONE', *, *, #7708, .F. ) ;
#2608 = ORIENTED_EDGE ( 'NONE', *, *, #657, .F. ) ;
#2609 = CARTESIAN_POINT ( 'NONE',  ( 49.86468353125001585, 38.75937500034139305, 16.20201782572375038 ) ) ;
#2610 = VERTEX_POINT ( 'NONE', #66 ) ;
#2611 = ORIENTED_EDGE ( 'NONE', *, *, #1818, .F. ) ;
#2612 = CARTESIAN_POINT ( 'NONE',  ( 25.75618375337248978, 283.9316295015381115, -8.256183753373985468 ) ) ;
#2613 = CARTESIAN_POINT ( 'NONE',  ( 49.86468353125001585, 48.75937500034140015, 16.20201782572375038 ) ) ;
#2614 = FACE_OUTER_BOUND ( 'NONE', #8305, .T. ) ;
#2615 = CARTESIAN_POINT ( 'NONE',  ( 15.40903463028482356, 26.52187500034139589, 47.42413220539093999 ) ) ;
#2616 = CYLINDRICAL_SURFACE ( 'NONE', #15808, 5.000000000000000000 ) ;
#2617 = AXIS2_PLACEMENT_3D ( 'NONE', #12532, #1125, #15100 ) ;
#2618 = CARTESIAN_POINT ( 'NONE',  ( -30.81806926056962226, 42.22187500034139163, 42.41743335407647919 ) ) ;
#2619 = CARTESIAN_POINT ( 'NONE',  ( -15.40903463028480580, 40.25937500034139305, 47.42413220539094709 ) ) ;
#2620 = CARTESIAN_POINT ( 'NONE',  ( -30.90169943749474513, 25.48125000068279888, -42.53254041760200721 ) ) ;
#2621 = CARTESIAN_POINT ( 'NONE',  ( 15.40903463028482356, 20.52187500034139589, 47.42413220539093999 ) ) ;
#2622 = CARTESIAN_POINT ( 'NONE',  ( -3.219174618344376363E-15, 27.28125000068279249, -52.57311121191334990 ) ) ;
#2623 = CARTESIAN_POINT ( 'NONE',  ( -15.45084971874737256, 35.38125000068279746, -47.55282581475767500 ) ) ;
#2624 = CARTESIAN_POINT ( 'NONE',  ( 40.34137639590981195, 31.12187500034139731, -29.30972558990011834 ) ) ;
#2625 = CARTESIAN_POINT ( 'NONE',  ( -49.99999999999999289, 28.10000000000000497, 16.24598481164533226 ) ) ;
#2626 = ORIENTED_EDGE ( 'NONE', *, *, #7947, .F. ) ;
#2627 = ORIENTED_EDGE ( 'NONE', *, *, #12849, .T. ) ;
#2628 = B_SPLINE_CURVE_WITH_KNOTS ( 'NONE', 3,
 ( #2987, #8056, #2736, #1497 ),
 .UNSPECIFIED., .F., .F.,
 ( 4, 4 ),
 ( 2.829004760679149478E-07, 0.001414802801989369172 ),
 .UNSPECIFIED. ) ;
#2629 = CARTESIAN_POINT ( 'NONE',  ( -12.16951863902676223, 34.13030016454078464, 101.6666710451724214 ) ) ;
#2630 = CARTESIAN_POINT ( 'NONE',  ( -0.5000000000000000000, 242.0000000000000284, 47.99999999999999289 ) ) ;
#2631 = CARTESIAN_POINT ( 'NONE',  ( -7.919222016226934890, 24.44874571845315714, 49.99999999999996447 ) ) ;
#2632 = CARTESIAN_POINT ( 'NONE',  ( -30.27664397204038593, 25.00000000000000355, 26.14048258526057467 ) ) ;
#2633 = CARTESIAN_POINT ( 'NONE',  ( 30.81806926056964002, 34.55937500034139731, 42.41743335407647209 ) ) ;
#2634 = CARTESIAN_POINT ( 'NONE',  ( 9.631387414534489405E-15, 44.42187500034140157, 52.43083105670540789 ) ) ;
#2635 =( GEOMETRIC_REPRESENTATION_CONTEXT ( 3 ) GLOBAL_UNCERTAINTY_ASSIGNED_CONTEXT ( ( #12754 ) ) GLOBAL_UNIT_ASSIGNED_CONTEXT ( ( #15017, #15102, #1127 ) ) REPRESENTATION_CONTEXT ( 'NONE', 'WORKASPACE' ) );
#2636 =( NAMED_UNIT ( * ) SI_UNIT ( $, .STERADIAN. ) SOLID_ANGLE_UNIT ( ) );
#2637 = CARTESIAN_POINT ( 'NONE',  ( 0.000000000000000000, 50.00000000000000000, -85.01963570546854498 ) ) ;
#2638 = CARTESIAN_POINT ( 'NONE',  ( -30.90169943749474513, 35.48125000068279888, -42.53254041760200721 ) ) ;
#2639 = LINE ( 'NONE', #5248, #7511 ) ;
#2640 = ORIENTED_EDGE ( 'NONE', *, *, #9573, .F. ) ;
#2641 = ADVANCED_FACE ( 'NONE', ( #15122 ), #15043, .T. ) ;
#2642 = CARTESIAN_POINT ( 'NONE',  ( 30.81806926056962936, 21.15937500034140228, -42.41743335407647209 ) ) ;
#2643 = ORIENTED_EDGE ( 'NONE', *, *, #11408, .F. ) ;
#2644 = FACE_OUTER_BOUND ( 'NONE', #11195, .T. ) ;
#2645 = ORIENTED_EDGE ( 'NONE', *, *, #3926, .T. ) ;
#2646 = VERTEX_POINT ( 'NONE', #9064 ) ;
#2647 = VECTOR ( 'NONE', #4240, 1000.000000000000000 ) ;
#2648 = CARTESIAN_POINT ( 'NONE',  ( 0.5000000000000009992, 31.99999999999998579, 101.0000000000000000 ) ) ;
#2649 = CARTESIAN_POINT ( 'NONE',  ( 2.464234863135679188, 13.31155363843775064, 102.0000000000000142 ) ) ;
#2650 = EDGE_CURVE ( 'NONE', #8967, #13787, #2656, .T. ) ;
#2651 = EDGE_CURVE ( 'NONE', #15408, #1769, #15198, .T. ) ;
#2652 = CARTESIAN_POINT ( 'NONE',  ( 7.919222016226809657, 29.44874571845315359, -50.00000000000000000 ) ) ;
#2653 = CARTESIAN_POINT ( 'NONE',  ( 48.98979485566355407, 261.9999999999999432, 10.00000000000000178 ) ) ;
#2654 = CARTESIAN_POINT ( 'NONE',  ( -5.988468393965924008, 15.10823117958422301, 102.0000000000000142 ) ) ;
#2655 = DIRECTION ( 'NONE',  ( 0.8090169943749505599, -0.5877852522924688072, -0.000000000000000000 ) ) ;
#2656 = LINE ( 'NONE', #16381, #6623 ) ;
#2657 = EDGE_CURVE ( 'NONE', #5002, #2769, #8724, .T. ) ;
#2658 = FACE_OUTER_BOUND ( 'NONE', #15932, .T. ) ;
#2659 = CARTESIAN_POINT ( 'NONE',  ( 30.90169943749474157, 41.08125000068280031, -42.53254041760200721 ) ) ;
#2660 = DIRECTION ( 'NONE',  ( 0.000000000000000000, 0.000000000000000000, -1.000000000000000000 ) ) ;
#2661 = ADVANCED_FACE ( 'NONE', ( #5016 ), #1490, .F. ) ;
#2662 = CARTESIAN_POINT ( 'NONE',  ( 9.657523855033129090E-15, 24.50000000000000355, 52.57311121191334990 ) ) ;
#2663 = CARTESIAN_POINT ( 'NONE',  ( -6.658212670116278709, 38.68388717334321569, 101.0000000000000000 ) ) ;
#2664 = VERTEX_POINT ( 'NONE', #7730 ) ;
#2665 = CARTESIAN_POINT ( 'NONE',  ( -30.81806926056962226, 44.15937500034139163, 42.41743335407647919 ) ) ;
#2666 = ORIENTED_EDGE ( 'NONE', *, *, #4217, .F. ) ;
#2667 = CARTESIAN_POINT ( 'NONE',  ( 7.919222016226809657, 43.22999571913594963, -50.00000000000000000 ) ) ;
#2668 = CARTESIAN_POINT ( 'NONE',  ( 0.000000000000000000, 20.00000000000000355, 0.000000000000000000 ) ) ;
#2670 = CARTESIAN_POINT ( 'NONE',  ( 15.40903463028482356, 26.45937500034139589, 47.42413220539093999 ) ) ;
#2669 =( BOUNDED_CURVE ( )  B_SPLINE_CURVE ( 2, ( #4867, #12420, #4695, #8575, #13399, #3350, #1011, #7017, #12163, #8424, #7107, #9923, #2094 ),
 .UNSPECIFIED., .F., .F. ) 
 B_SPLINE_CURVE_WITH_KNOTS ( ( 3, 2, 2, 2, 2, 2, 3 ),
 ( 0.4833333333333333370, 0.4866666666666666918, 0.4933333333333333459, 0.5000000000000000000, 0.5066666666666667096, 0.5133333333333333082, 0.5166666666666667185 ),
 .UNSPECIFIED. ) 
 CURVE ( )  GEOMETRIC_REPRESENTATION_ITEM ( )  RATIONAL_B_SPLINE_CURVE ( ( 0.9755282581475768211, 0.9755282581475768211, 1.000000000000000000, 0.9510565162951535312, 1.000000000000000000, 0.9510565162951535312, 1.000000000000000000, 0.9510565162951535312, 1.000000000000000000, 0.9510565162951535312, 1.000000000000000000, 0.9755282581475763770, 0.9755282581475768211 ) ) 
 REPRESENTATION_ITEM ( '' )  );
#2671 = ORIENTED_EDGE ( 'NONE', *, *, #15404, .T. ) ;
#2672 = CARTESIAN_POINT ( 'NONE',  ( 30.90169943749475223, 32.70000000000000284, 42.53254041760199300 ) ) ;
#2673 = DIRECTION ( 'NONE',  ( 0.000000000000000000, 0.000000000000000000, 1.000000000000000000 ) ) ;
#2674 = CARTESIAN_POINT ( 'NONE',  ( 47.24032962522667134, 25.00000000000000711, -15.96451374291363301 ) ) ;
#2675 = CARTESIAN_POINT ( 'NONE',  ( -49.86468353124999453, 31.82187500034139305, -16.20201782572375393 ) ) ;
#2676 = CARTESIAN_POINT ( 'NONE',  ( 15.45084971874737789, 30.38125000068280102, 47.55282581475767500 ) ) ;
#2677 = CARTESIAN_POINT ( 'NONE',  ( -30.81806926056963292, 23.55937500034139376, -42.41743335407646498 ) ) ;
#2678 = FACE_OUTER_BOUND ( 'NONE', #15899, .T. ) ;
#2679 = CARTESIAN_POINT ( 'NONE',  ( 9.631387414534489405E-15, 30.42187500034139447, 52.43083105670540789 ) ) ;
#2680 = CARTESIAN_POINT ( 'NONE',  ( 0.000000000000000000, 52.00000000000000711, 65.00000000000000000 ) ) ;
#2681 = CARTESIAN_POINT ( 'NONE',  ( 49.99999999999999289, 31.09999999999999787, -16.24598481164532160 ) ) ;
#2682 = CARTESIAN_POINT ( 'NONE',  ( -40.34137639590981905, 31.65937500034139873, -29.30972558990011478 ) ) ;
#2683 = CARTESIAN_POINT ( 'NONE',  ( -49.86468353124999453, 34.02187500034140299, 16.20201782572377525 ) ) ;
#2684 = CARTESIAN_POINT ( 'NONE',  ( 30.90169943749474157, 41.30000000000001137, -42.53254041760200721 ) ) ;
#2685 = ORIENTED_EDGE ( 'NONE', *, *, #12100, .T. ) ;
#2686 = CARTESIAN_POINT ( 'NONE',  ( 30.81806926056964002, 36.55937500034139731, 42.41743335407646498 ) ) ;
#2687 = ORIENTED_EDGE ( 'NONE', *, *, #12513, .T. ) ;
#2688 = ORIENTED_EDGE ( 'NONE', *, *, #3686, .T. ) ;
#2689 = CARTESIAN_POINT ( 'NONE',  ( 25.66084200510924518, 284.4942466289054437, -3.821684010228425077 ) ) ;
#2690 = CARTESIAN_POINT ( 'NONE',  ( 49.86468353124999453, 46.95937500034139589, -16.20201782572376459 ) ) ;
#2691 = DIRECTION ( 'NONE',  ( 0.9781476007338041345, 0.2079116908177665313, 0.000000000000000000 ) ) ;
#2692 = CARTESIAN_POINT ( 'NONE',  ( 49.86468353124999453, 25.02187500034139589, -16.20201782572376459 ) ) ;
#2693 = DIRECTION ( 'NONE',  ( 0.000000000000000000, -0.000000000000000000, 1.000000000000000000 ) ) ;
#2694 = CARTESIAN_POINT ( 'NONE',  ( -49.86468353125000164, 39.92187500034139447, 0.000000000000000000 ) ) ;
#2695 = CARTESIAN_POINT ( 'NONE',  ( -30.81806926056963292, 45.55937500034139731, -42.41743335407646498 ) ) ;
#2696 = CARTESIAN_POINT ( 'NONE',  ( -5.823736356558307894E-14, 44.50000000000000000, 50.00000000000000000 ) ) ;
#2697 = CARTESIAN_POINT ( 'NONE',  ( 15.45084971874737789, 44.60000000000000142, 47.55282581475767500 ) ) ;
#2698 = ADVANCED_FACE ( 'NONE', ( #153 ), #3746, .T. ) ;
#2699 = CARTESIAN_POINT ( 'NONE',  ( -3.219174618344376363E-15, 25.28125000068279604, -52.57311121191334990 ) ) ;
#2700 = CARTESIAN_POINT ( 'NONE',  ( 8.787474317778430688, 37.67774414662245164, 92.94678285709053966 ) ) ;
#2701 = CARTESIAN_POINT ( 'NONE',  ( 30.81806926056962936, 29.22187500034139873, -42.41743335407647209 ) ) ;
#2702 = CARTESIAN_POINT ( 'NONE',  ( -3.111920190527341144E-15, 27.50000000000000000, -50.00000000000000000 ) ) ;
#2703 = VERTEX_POINT ( 'NONE', #12553 ) ;
#2704 = CARTESIAN_POINT ( 'NONE',  ( -30.90169943749474868, 37.48125000068279888, -42.53254041760200721 ) ) ;
#2705 = ORIENTED_EDGE ( 'NONE', *, *, #4334, .F. ) ;
#2706 = DIRECTION ( 'NONE',  ( 0.9945218953682730678, 0.1045284632676572317, 0.000000000000000000 ) ) ;
#2707 = CARTESIAN_POINT ( 'NONE',  ( 15.11046079763426420, 14.35332166009638222, 101.3333374614808662 ) ) ;
#2708 = DIRECTION ( 'NONE',  ( -0.3535533905932727872, -0.7071067811865462405, 0.6123724356957966908 ) ) ;
#2709 = CARTESIAN_POINT ( 'NONE',  ( -3.210462471511496205E-15, 49.42187500034138736, -52.43083105670540789 ) ) ;
#2710 = CARTESIAN_POINT ( 'NONE',  ( -49.86468353124999453, 31.95937500034139944, 16.20201782572377525 ) ) ;
#2711 = CARTESIAN_POINT ( 'NONE',  ( 0.000000000000000000, 0.000000000000000000, -5.000000000000000000 ) ) ;
#2712 = CARTESIAN_POINT ( 'NONE',  ( 40.34137639590981905, 44.72187500034139163, 29.30972558990010768 ) ) ;
#2713 = APPLICATION_PROTOCOL_DEFINITION ( 'draft international standard', 'automotive_design', 1998, #16090 ) ;
#2714 = CARTESIAN_POINT ( 'NONE',  ( 15.45084971874737789, 34.38125000068280457, 47.55282581475767500 ) ) ;
#2715 = PLANE ( 'NONE',  #8699 ) ;
#2716 = DIRECTION ( 'NONE',  ( 0.9961946980917455452, 0.08715574274765824914, 0.000000000000000000 ) ) ;
#2717 = ORIENTED_EDGE ( 'NONE', *, *, #13322, .F. ) ;
#2718 = AXIS2_PLACEMENT_3D ( 'NONE', #10721, #12040, #4408 ) ;
#2719 = CARTESIAN_POINT ( 'NONE',  ( -15.40903463028480580, 46.32187500034140015, 47.42413220539094709 ) ) ;
#2720 = ORIENTED_EDGE ( 'NONE', *, *, #4595, .F. ) ;
#2721 = CARTESIAN_POINT ( 'NONE',  ( 6.123233995736766085E-15, 20.00000000000000355, -50.00000000000000000 ) ) ;
#2722 = ORIENTED_EDGE ( 'NONE', *, *, #1549, .T. ) ;
#2723 = ORIENTED_EDGE ( 'NONE', *, *, #4292, .F. ) ;
#2724 = EDGE_CURVE ( 'NONE', #3391, #5387, #4786, .T. ) ;
#2725 = CYLINDRICAL_SURFACE ( 'NONE', #2306, 60.00000000000000711 ) ;
#2726 = FACE_OUTER_BOUND ( 'NONE', #6080, .T. ) ;
#2727 = CARTESIAN_POINT ( 'NONE',  ( 7.919222016226822092, 28.55125428154684286, 49.99999999999999289 ) ) ;
#2728 = CARTESIAN_POINT ( 'NONE',  ( 50.00000000000000711, 26.89999999999999503, 16.24598481164530739 ) ) ;
#2729 = DIRECTION ( 'NONE',  ( -0.000000000000000000, -0.000000000000000000, -1.000000000000000000 ) ) ;
#2730 = CARTESIAN_POINT ( 'NONE',  ( 2.600676159226421000E-13, 31.49999999999999289, -49.99999999999999289 ) ) ;
#2731 = CARTESIAN_POINT ( 'NONE',  ( -49.99999999999999289, 25.68125000068279817, -16.24598481164531449 ) ) ;
#2732 = CARTESIAN_POINT ( 'NONE',  ( 50.00000000000000711, 24.68125000068279462, 16.24598481164530739 ) ) ;
#2733 = VECTOR ( 'NONE', #7619, 1000.000000000000000 ) ;
#2734 = CARTESIAN_POINT ( 'NONE',  ( 40.45084971874737789, 48.80000000000000426, 29.38926261462365375 ) ) ;
#2735 = CARTESIAN_POINT ( 'NONE',  ( 15.45084971874736723, 41.18125000068280173, -47.55282581475768211 ) ) ;
#2736 = CARTESIAN_POINT ( 'NONE',  ( 16.15689471564400037, 27.22396221095515045, 101.6666710451724214 ) ) ;
#2737 = CARTESIAN_POINT ( 'NONE',  ( -15.45084971874737256, 21.60000000000000142, -47.55282581475767500 ) ) ;
#2738 = DIRECTION ( 'NONE',  ( -1.000000000000000000, 0.000000000000000000, -0.000000000000000000 ) ) ;
#2739 = EDGE_CURVE ( 'NONE', #40, #9078, #689, .T. ) ;
#2740 = PRODUCT_DEFINITION ( 'UNKNOWN', '', #6278, #2088 ) ;
#2741 = VERTEX_POINT ( 'NONE', #556 ) ;
#2742 = CARTESIAN_POINT ( 'NONE',  ( -40.34137639590981905, 37.65937500034139873, -29.30972558990011478 ) ) ;
#2743 = VERTEX_POINT ( 'NONE', #14364 ) ;
#2744 = AXIS2_PLACEMENT_3D ( 'NONE', #14436, #2907, #2821 ) ;
#2745 = DIRECTION ( 'NONE',  ( 0.000000000000000000, 0.000000000000000000, 1.000000000000000000 ) ) ;
#2746 = EDGE_CURVE ( 'NONE', #3704, #798, #10472, .T. ) ;
#2747 = CARTESIAN_POINT ( 'NONE',  ( -8.660254037844387298, 20.00000000000000355, 5.000000000000000000 ) ) ;
#2748 = CARTESIAN_POINT ( 'NONE',  ( -49.86468353124999453, 29.75937500034139305, -16.20201782572375393 ) ) ;
#2749 = EDGE_LOOP ( 'NONE', ( #3498, #3015, #13277, #12584 ) ) ;
#2750 = CARTESIAN_POINT ( 'NONE',  ( 30.90169943749475223, 26.70000000000000284, 42.53254041760199300 ) ) ;
#2751 = FACE_OUTER_BOUND ( 'NONE', #7948, .T. ) ;
#2752 = LINE ( 'NONE', #3085, #16275 ) ;
#2753 = CARTESIAN_POINT ( 'NONE',  ( 15.40903463028482356, 36.52187500034139589, 47.42413220539093999 ) ) ;
#2754 = EDGE_CURVE ( 'NONE', #2831, #2833, #13123, .T. ) ;
#2755 = CARTESIAN_POINT ( 'NONE',  ( -40.45084971874737079, 29.98125000068279888, 29.38926261462367151 ) ) ;
#2756 = CARTESIAN_POINT ( 'NONE',  ( -40.34137639590981195, 24.05937500034139731, 29.30972558990012189 ) ) ;
#2757 = CARTESIAN_POINT ( 'NONE',  ( -1.224646799147353217E-14, 0.000000000000000000, -100.0000000000000000 ) ) ;
#2758 = CARTESIAN_POINT ( 'NONE',  ( -49.86468353124999453, 32.02187500034139589, 16.20201782572377169 ) ) ;
#2759 = DIRECTION ( 'NONE',  ( 1.734723475976807094E-17, 0.000000000000000000, -1.000000000000000000 ) ) ;
#2760 = AXIS2_PLACEMENT_3D ( 'NONE', #1402, #1075, #7654 ) ;
#2761 = CARTESIAN_POINT ( 'NONE',  ( -49.99999999999999289, 34.10000000000000853, 16.24598481164533226 ) ) ;
#2762 = CARTESIAN_POINT ( 'NONE',  ( 30.81806926056962936, 31.15937500034139518, -42.41743335407647209 ) ) ;
#2763 = CARTESIAN_POINT ( 'NONE',  ( -40.34137639590981195, 34.12187500034139731, 29.30972558990012189 ) ) ;
#2764 = ORIENTED_EDGE ( 'NONE', *, *, #3779, .F. ) ;
#2765 =( BOUNDED_CURVE ( )  B_SPLINE_CURVE ( 3, ( #5034, #10086, #15136, #3763 ),
 .UNSPECIFIED., .F., .F. ) 
 B_SPLINE_CURVE_WITH_KNOTS ( ( 4, 4 ),
 ( 4.523772594209285458, 4.901005366560093002 ),
 .UNSPECIFIED. ) 
 CURVE ( )  GEOMETRIC_REPRESENTATION_ITEM ( )  RATIONAL_B_SPLINE_CURVE ( ( 1.000000000000000000, 0.9881764018959044993, 0.9881764018959044993, 1.000000000000000000 ) ) 
 REPRESENTATION_ITEM ( '' )  );
#2766 = EDGE_CURVE ( 'NONE', #16188, #14047, #10606, .T. ) ;
#2767 = PRODUCT_DEFINITION_CONTEXT ( 'detailed design', #16090, 'design' ) ;
#2768 = CARTESIAN_POINT ( 'NONE',  ( -30.81806926056963292, 37.55937500034139020, -42.41743335407646498 ) ) ;
#2769 = VERTEX_POINT ( 'NONE', #15775 ) ;
#2770 = CARTESIAN_POINT ( 'NONE',  ( 26.40559293885987557, 283.2826504366940412, -8.905592938858417185 ) ) ;
#2771 = CARTESIAN_POINT ( 'NONE',  ( -30.81806926056963292, 49.55937500034139731, -42.41743335407647209 ) ) ;
#2772 = CIRCLE ( 'NONE', #12062, 50.00000000000000000 ) ;
#2773 = CARTESIAN_POINT ( 'NONE',  ( 2.499999999999999556, 242.0000000000000284, 49.17157287525379417 ) ) ;
#2774 = CARTESIAN_POINT ( 'NONE',  ( -40.34137639590981195, 24.12187500034139731, 29.30972558990012189 ) ) ;
#2775 = EDGE_CURVE ( 'NONE', #9017, #306, #15530, .T. ) ;
#2776 = CARTESIAN_POINT ( 'NONE',  ( -23.39173249367811636, 283.2330659413077001, 9.195866246826893686 ) ) ;
#2777 = CARTESIAN_POINT ( 'NONE',  ( -49.86468353124999453, 37.82187500034139305, -16.20201782572375393 ) ) ;
#2778 = CARTESIAN_POINT ( 'NONE',  ( 49.86468353125001585, 44.75937500034139305, 16.20201782572375038 ) ) ;
#2779 = DIRECTION ( 'NONE',  ( -0.9945218953682744001, 0.1045284632676435205, 0.000000000000000000 ) ) ;
#2780 = CARTESIAN_POINT ( 'NONE',  ( -30.90169943749474868, 47.70000000000000995, -42.53254041760200721 ) ) ;
#2781 = CARTESIAN_POINT ( 'NONE',  ( -49.86468353125000164, 49.85937500034139447, 0.000000000000000000 ) ) ;
#2782 = LINE ( 'NONE', #11604, #16387 ) ;
#2783 = MECHANICAL_DESIGN_GEOMETRIC_PRESENTATION_REPRESENTATION (  '', ( #4121 ), #12873 ) ;
#2784 = CARTESIAN_POINT ( 'NONE',  ( -49.86468353125000164, 29.92187500034139802, 0.000000000000000000 ) ) ;
#2785 = EDGE_CURVE ( 'NONE', #10405, #10911, #9472, .T. ) ;
#2786 = DIRECTION ( 'NONE',  ( -0.000000000000000000, -1.000000000000000000, -0.000000000000000000 ) ) ;
#2787 = ORIENTED_EDGE ( 'NONE', *, *, #12706, .F. ) ;
#2788 = CARTESIAN_POINT ( 'NONE',  ( -50.00000000000000000, 37.78125000068280315, 0.000000000000000000 ) ) ;
#2789 = ORIENTED_EDGE ( 'NONE', *, *, #16426, .T. ) ;
#2790 = DIRECTION ( 'NONE',  ( -1.000000000000000000, 0.000000000000000000, -2.602085213965210149E-16 ) ) ;
#2791 = DIRECTION ( 'NONE',  ( 0.000000000000000000, 8.780190904559502465E-17, 1.000000000000000000 ) ) ;
#2792 = VECTOR ( 'NONE', #7140, 1000.000000000000000 ) ;
#2793 = CARTESIAN_POINT ( 'NONE',  ( -15.39925740754308059, 14.18658485962419569, 101.0000000000000000 ) ) ;
#2794 = CARTESIAN_POINT ( 'NONE',  ( -3.210462471511496205E-15, 47.42187500034138736, -52.43083105670540789 ) ) ;
#2795 = CARTESIAN_POINT ( 'NONE',  ( 49.86468353125001585, 22.75937500034139660, 16.20201782572375038 ) ) ;
#2796 = PRESENTATION_LAYER_ASSIGNMENT (  '', '', ( #661 ) ) ;
#2797 = CARTESIAN_POINT ( 'NONE',  ( 24.78626291527397285, 40.00000000000000711, 5.650101528493621572 ) ) ;
#2798 = CARTESIAN_POINT ( 'NONE',  ( -30.81806926056963292, 43.62187500034139020, -42.41743335407646498 ) ) ;
#2799 = CARTESIAN_POINT ( 'NONE',  ( 0.000000000000000000, 0.000000000000000000, 0.000000000000000000 ) ) ;
#2800 = CARTESIAN_POINT ( 'NONE',  ( -15.40903463028480580, 46.32187500034140015, 47.42413220539094709 ) ) ;
#2801 = CARTESIAN_POINT ( 'NONE',  ( 0.000000000000000000, 267.0000000000000000, 45.00000000000000000 ) ) ;
#2802 = AXIS2_PLACEMENT_3D ( 'NONE', #13583, #2111, #14828 ) ;
#2803 = ORIENTED_EDGE ( 'NONE', *, *, #2952, .F. ) ;
#2804 = VECTOR ( 'NONE', #1089, 1000.000000000000000 ) ;
#2805 = CARTESIAN_POINT ( 'NONE',  ( -3.210462471511496205E-15, 47.42187500034138736, -52.43083105670540789 ) ) ;
#2806 = PRODUCT ( 'BR-819', 'BR-819', '', ( #5395 ) ) ;
#2807 = ORIENTED_EDGE ( 'NONE', *, *, #10077, .T. ) ;
#2808 = CARTESIAN_POINT ( 'NONE',  ( -0.5000000000000000000, 39.99285568453590400, 101.0000000000000000 ) ) ;
#2809 = EDGE_LOOP ( 'NONE', ( #5254, #6057, #13537, #8063 ) ) ;
#2810 = VERTEX_POINT ( 'NONE', #4162 ) ;
#2811 = AXIS2_PLACEMENT_3D ( 'NONE', #4307, #11942, #9372 ) ;
#2812 = AXIS2_PLACEMENT_3D ( 'NONE', #8014, #12076, #15734 ) ;
#2813 = CARTESIAN_POINT ( 'NONE',  ( -2.500000000000000000, 242.0000000000000284, 40.00000000000000000 ) ) ;
#2814 = DIRECTION ( 'NONE',  ( -0.000000000000000000, -1.000000000000000000, -0.000000000000000000 ) ) ;
#2815 = FILL_AREA_STYLE_COLOUR ( '', #1312 ) ;
#2816 = CARTESIAN_POINT ( 'NONE',  ( -40.45084971874737789, 27.80000000000000071, -29.38926261462365730 ) ) ;
#2817 = AXIS2_PLACEMENT_3D ( 'NONE', #3359, #1931, #7024 ) ;
#2818 = CARTESIAN_POINT ( 'NONE',  ( 30.81806926056962936, 47.15937500034138452, -42.41743335407647209 ) ) ;
#2819 = CONICAL_SURFACE ( 'NONE', #3355, 16.50000000000000711, 0.7853981633974447263 ) ;
#2820 = CIRCLE ( 'NONE', #681, 2.000000000000001776 ) ;
#2821 = DIRECTION ( 'NONE',  ( 0.000000000000000000, 0.000000000000000000, 1.000000000000000000 ) ) ;
#2822 = DIRECTION ( 'NONE',  ( 0.000000000000000000, 0.6143407043256605693, -0.7890408728378088821 ) ) ;
#2823 = VECTOR ( 'NONE', #5091, 1000.000000000000114 ) ;
#2824 = CARTESIAN_POINT ( 'NONE',  ( -15.40903463028481646, 21.52187500034139589, -47.42413220539093999 ) ) ;
#2825 = FILL_AREA_STYLE ('',( #481 ) ) ;
#2826 = CARTESIAN_POINT ( 'NONE',  ( -5.988468393965924008, 15.10823117958422301, 101.0000000000000000 ) ) ;
#2827 = CARTESIAN_POINT ( 'NONE',  ( -15.45084971874737256, 37.38125000068279746, -47.55282581475767500 ) ) ;
#2828 = LINE ( 'NONE', #14121, #4187 ) ;
#2829 = DIRECTION ( 'NONE',  ( 0.000000000000000000, 1.000000000000000000, 0.000000000000000000 ) ) ;
#2830 =( NAMED_UNIT ( * ) SI_UNIT ( $, .STERADIAN. ) SOLID_ANGLE_UNIT ( ) );
#2831 = VERTEX_POINT ( 'NONE', #4322 ) ;
#2832 = CARTESIAN_POINT ( 'NONE',  ( -30.81806926056962226, 40.15937500034139163, 42.41743335407647919 ) ) ;
#2833 = VERTEX_POINT ( 'NONE', #2981 ) ;
#2834 = VECTOR ( 'NONE', #14855, 1000.000000000000000 ) ;
#2835 = VECTOR ( 'NONE', #5105, 1000.000000000000000 ) ;
#2836 = CARTESIAN_POINT ( 'NONE',  ( -15.45084971874737256, 49.38125000068280457, -47.55282581475767500 ) ) ;
#2837 = DIRECTION ( 'NONE',  ( -0.7431448254773861395, -0.6691306063588672304, 0.000000000000000000 ) ) ;
#2838 = CARTESIAN_POINT ( 'NONE',  ( 30.81806926056962936, 25.15937500034139518, -42.41743335407647209 ) ) ;
#2839 = EDGE_LOOP ( 'NONE', ( #1252, #10363, #14918, #2723 ) ) ;
#2840 = DIRECTION ( 'NONE',  ( 0.000000000000000000, 0.000000000000000000, 1.000000000000000000 ) ) ;
#2842 = EDGE_CURVE ( 'NONE', #2273, #10236, #11393, .T. ) ;
#2841 = CARTESIAN_POINT ( 'NONE',  ( -11.57407943811421802, 35.63861574361248330, 92.99953801807581044 ) ) ;
#2843 = CARTESIAN_POINT ( 'NONE',  ( -4.999999999999930722, 107.2206331336082741, -16.63484669598130949 ) ) ;
#2844 = CARTESIAN_POINT ( 'NONE',  ( -40.34137639590981905, 29.72187500034139518, -29.30972558990011478 ) ) ;
#2845 = CARTESIAN_POINT ( 'NONE',  ( -15.45084971874737256, 29.38125000068279746, -47.55282581475767500 ) ) ;
#2846 = AXIS2_PLACEMENT_3D ( 'NONE', #2083, #11076, #664 ) ;
#2847 = CARTESIAN_POINT ( 'NONE',  ( 2.894151059106554236, 5.231075460314085213, 99.03700517889676291 ) ) ;
#2848 = CARTESIAN_POINT ( 'NONE',  ( -46.79661121261588619, 20.00000000000000355, 17.22183559214931492 ) ) ;
#2849 = CARTESIAN_POINT ( 'NONE',  ( -49.86468353124999453, 28.02187500034139589, 16.20201782572377169 ) ) ;
#2850 = VECTOR ( 'NONE', #5336, 1000.000000000000000 ) ;
#2851 = DIRECTION ( 'NONE',  ( 0.000000000000000000, 0.000000000000000000, -1.000000000000000000 ) ) ;
#2852 = CARTESIAN_POINT ( 'NONE',  ( -49.99999999999999289, 31.89999999999999858, -16.24598481164531449 ) ) ;
#2853 = CARTESIAN_POINT ( 'NONE',  ( 49.86468353125001585, 32.75937500034140015, 16.20201782572375038 ) ) ;
#2854 = CARTESIAN_POINT ( 'NONE',  ( -49.86468353125000164, 27.92187500034139447, 0.000000000000000000 ) ) ;
#2855 = LINE ( 'NONE', #9172, #10962 ) ;
#2856 = ORIENTED_EDGE ( 'NONE', *, *, #11284, .F. ) ;
#2857 = ADVANCED_FACE ( 'NONE', ( #9140 ), #236, .F. ) ;
#2858 = CARTESIAN_POINT ( 'NONE',  ( -15.40903463028481646, 27.45937500034139944, -47.42413220539093999 ) ) ;
#2859 = ORIENTED_EDGE ( 'NONE', *, *, #8927, .T. ) ;
#2860 = CARTESIAN_POINT ( 'NONE',  ( 29.67274705320743777, 282.0000000000000000, -11.84549410641326084 ) ) ;
#2861 = CARTESIAN_POINT ( 'NONE',  ( 40.34137639590981905, 48.65937500034139873, 29.30972558990010768 ) ) ;
#2862 = EDGE_CURVE ( 'NONE', #8967, #11302, #6358, .T. ) ;
#2863 = CYLINDRICAL_SURFACE ( 'NONE', #14977, 50.00000000000000000 ) ;
#2864 = CARTESIAN_POINT ( 'NONE',  ( 30.81806926056964002, 20.62187500034139020, 42.41743335407647209 ) ) ;
#2865 = ADVANCED_FACE ( 'NONE', ( #4401 ), #14826, .T. ) ;
#2866 = FACE_OUTER_BOUND ( 'NONE', #2972, .T. ) ;
#2867 = CARTESIAN_POINT ( 'NONE',  ( -30.81806926056963292, 33.62187500034139731, -42.41743335407647209 ) ) ;
#2868 = CARTESIAN_POINT ( 'NONE',  ( 49.86468353125000164, 32.85937500034139447, -6.106662507704105588E-15 ) ) ;
#2869 = DIRECTION ( 'NONE',  ( 0.1045284632676436176, 0.9945218953682742891, 0.000000000000000000 ) ) ;
#2870 = CARTESIAN_POINT ( 'NONE',  ( 9.657523855033129090E-15, 38.50000000000000711, 52.57311121191334990 ) ) ;
#2871 = ADVANCED_FACE ( 'NONE', ( #5500 ), #2908, .F. ) ;
#2872 = CARTESIAN_POINT ( 'NONE',  ( 30.90169943749474157, 23.08125000068279320, -42.53254041760200721 ) ) ;
#2873 = CARTESIAN_POINT ( 'NONE',  ( 49.86468353125000164, 44.92187500034140157, -6.106662507704105588E-15 ) ) ;
#2874 =( BOUNDED_CURVE ( )  B_SPLINE_CURVE ( 2, ( #4425, #5597, #1904, #13304, #498, #4342, #8070, #334, #8161, #9407, #10494, #3084, #4183 ),
 .UNSPECIFIED., .F., .F. ) 
 B_SPLINE_CURVE_WITH_KNOTS ( ( 3, 2, 2, 2, 2, 2, 3 ),
 ( 0.8833333333333334147, 0.8866666666666667140, 0.8933333333333333126, 0.9000000000000000222, 0.9066666666666666208, 0.9133333333333333304, 0.9166666666666667407 ),
 .UNSPECIFIED. ) 
 CURVE ( )  GEOMETRIC_REPRESENTATION_ITEM ( )  RATIONAL_B_SPLINE_CURVE ( ( 0.9755282581475768211, 0.9755282581475771542, 1.000000000000000000, 0.9510565162951535312, 1.000000000000000000, 0.9510565162951535312, 1.000000000000000000, 0.9510565162951535312, 1.000000000000000000, 0.9510565162951535312, 1.000000000000000000, 0.9755282581475763770, 0.9755282581475768211 ) ) 
 REPRESENTATION_ITEM ( '' )  );
#2875 = CARTESIAN_POINT ( 'NONE',  ( 9.631387414534489405E-15, 28.42187500034139092, 52.43083105670540789 ) ) ;
#2876 = CARTESIAN_POINT ( 'NONE',  ( 16.34981105473766760, 20.27881147257189909, 102.0000000000000142 ) ) ;
#2877 = ORIENTED_EDGE ( 'NONE', *, *, #2842, .F. ) ;
#2878 = CARTESIAN_POINT ( 'NONE',  ( -50.00000000000000000, 35.78125000068280315, 0.000000000000000000 ) ) ;
#2879 = AXIS2_PLACEMENT_3D ( 'NONE', #14621, #11236, #5920 ) ;
#2880 = VERTEX_POINT ( 'NONE', #6665 ) ;
#2881 = DIRECTION ( 'NONE',  ( -1.000000000000000000, 0.000000000000000000, 0.000000000000000000 ) ) ;
#2882 = DIRECTION ( 'NONE',  ( -0.000000000000000000, -1.000000000000000000, -0.000000000000000000 ) ) ;
#2883 = CARTESIAN_POINT ( 'NONE',  ( 7.919222016226693306, 30.33250428222964246, 50.00000000000003553 ) ) ;
#2884 = CARTESIAN_POINT ( 'NONE',  ( -49.86468353124999453, 47.82187500034140015, -16.20201782572375393 ) ) ;
#2885 = CARTESIAN_POINT ( 'NONE',  ( -49.86468353125000164, 21.85937500034139802, 0.000000000000000000 ) ) ;
#2886 = ADVANCED_FACE ( 'NONE', ( #14199, #11958 ), #12968, .F. ) ;
#2887 = DIRECTION ( 'NONE',  ( 0.000000000000000000, 0.000000000000000000, 1.000000000000000000 ) ) ;
#2888 = CARTESIAN_POINT ( 'NONE',  ( 49.86468353124999453, 43.02187500034138878, -16.20201782572376104 ) ) ;
#2889 = CARTESIAN_POINT ( 'NONE',  ( 0.000000000000000000, 0.000000000000000000, 0.000000000000000000 ) ) ;
#2890 = DIRECTION ( 'NONE',  ( -0.000000000000000000, 1.000000000000000000, -0.000000000000000000 ) ) ;
#2891 = EDGE_CURVE ( 'NONE', #12805, #6547, #3145, .T. ) ;
#2892 = AXIS2_PLACEMENT_3D ( 'NONE', #9824, #14875, #2238 ) ;
#2893 = CARTESIAN_POINT ( 'NONE',  ( -49.86468353124999453, 48.02187500034139589, 16.20201782572377525 ) ) ;
#2894 = CARTESIAN_POINT ( 'NONE',  ( 8.446640517145639571E-15, 28.28125000068279959, 50.00000000000000000 ) ) ;
#2895 = ORIENTED_EDGE ( 'NONE', *, *, #7557, .F. ) ;
#2896 = CARTESIAN_POINT ( 'NONE',  ( -3.210462471511496205E-15, 45.42187500034139447, -52.43083105670540789 ) ) ;
#2897 = ORIENTED_EDGE ( 'NONE', *, *, #3232, .T. ) ;
#2898 = DIRECTION ( 'NONE',  ( -0.6691306063588671194, 0.7431448254773861395, 0.000000000000000000 ) ) ;
#2899 = ORIENTED_EDGE ( 'NONE', *, *, #2263, .T. ) ;
#2900 = ORIENTED_EDGE ( 'NONE', *, *, #9779, .F. ) ;
#2901 = CARTESIAN_POINT ( 'NONE',  ( -40.45084971874737079, 43.98125000068279888, 29.38926261462367151 ) ) ;
#2902 = CARTESIAN_POINT ( 'NONE',  ( 0.000000000000000000, 257.0000000000001137, 0.000000000000000000 ) ) ;
#2903 = DIRECTION ( 'NONE',  ( -0.000000000000000000, 1.000000000000000000, -0.000000000000000000 ) ) ;
#2904 = CARTESIAN_POINT ( 'NONE',  ( 50.00000000000000000, 27.00000000000000355, -6.123233995736766085E-15 ) ) ;
#2905 = VECTOR ( 'NONE', #3482, 1000.000000000000000 ) ;
#2906 = CARTESIAN_POINT ( 'NONE',  ( -49.86468353124999453, 41.75937500034139305, -16.20201782572375393 ) ) ;
#2907 = DIRECTION ( 'NONE',  ( -0.000000000000000000, 1.000000000000000000, -0.000000000000000000 ) ) ;
#2908 = PLANE ( 'NONE',  #12718 ) ;
#2909 = CARTESIAN_POINT ( 'NONE',  ( 0.000000000000000000, 312.0000000000000568, 0.000000000000000000 ) ) ;
#2910 = CARTESIAN_POINT ( 'NONE',  ( 30.90169943749475578, 40.48125000068279888, 42.53254041760200010 ) ) ;
#2911 = CARTESIAN_POINT ( 'NONE',  ( -7.919222016226752814, 37.33250428222964246, -50.00000000000000711 ) ) ;
#2912 = EDGE_CURVE ( 'NONE', #12041, #1101, #11793, .T. ) ;
#2913 = CARTESIAN_POINT ( 'NONE',  ( 7.919222016226693306, 22.33250428222964601, 50.00000000000003553 ) ) ;
#2914 = EDGE_CURVE ( 'NONE', #4422, #5607, #13285, .T. ) ;
#2915 = DIRECTION ( 'NONE',  ( -0.000000000000000000, 1.000000000000000000, -0.000000000000000000 ) ) ;
#2916 = ORIENTED_EDGE ( 'NONE', *, *, #14086, .F. ) ;
#2917 = CARTESIAN_POINT ( 'NONE',  ( -30.81806926056963292, 37.55937500034139020, -42.41743335407647209 ) ) ;
#2918 = ORIENTED_EDGE ( 'NONE', *, *, #4039, .T. ) ;
#2919 = ORIENTED_EDGE ( 'NONE', *, *, #826, .T. ) ;
#2920 = CARTESIAN_POINT ( 'NONE',  ( 40.45084971874737079, 46.98125000068280599, -29.38926261462366440 ) ) ;
#2921 = CYLINDRICAL_SURFACE ( 'NONE', #972, 40.00000000000000000 ) ;
#2922 = CARTESIAN_POINT ( 'NONE',  ( 49.86468353124999453, 24.95937500034139234, -16.20201782572376459 ) ) ;
#2923 = ORIENTED_EDGE ( 'NONE', *, *, #13600, .T. ) ;
#2924 = CARTESIAN_POINT ( 'NONE',  ( 1.235979693235591175E-19, 4.999999999999997335, 99.11836509645767990 ) ) ;
#2925 = PLANE ( 'NONE',  #10258 ) ;
#2926 = DIRECTION ( 'NONE',  ( 0.2079116908177531253, 0.9781476007338069101, 0.000000000000000000 ) ) ;
#2927 = CARTESIAN_POINT ( 'NONE',  ( 49.86468353125001585, 26.82187500034139305, 16.20201782572375038 ) ) ;
#2928 = PLANE ( 'NONE',  #15020 ) ;
#2929 = CARTESIAN_POINT ( 'NONE',  ( 0.000000000000000000, 22.50000000000000000, 101.0000000000000000 ) ) ;
#2930 = CARTESIAN_POINT ( 'NONE',  ( -46.38089879718444308, 20.00000000000000355, 18.31192695794416636 ) ) ;
#2931 = CARTESIAN_POINT ( 'NONE',  ( 15.40903463028481113, 29.32187500034139660, -47.42413220539094709 ) ) ;
#2932 = CARTESIAN_POINT ( 'NONE',  ( 19.99999999999999645, 287.0000000000000568, 2.500000000000002220 ) ) ;
#2933 = CARTESIAN_POINT ( 'NONE',  ( -15.45084971874737256, 33.60000000000000142, -47.55282581475767500 ) ) ;
#2934 = CARTESIAN_POINT ( 'NONE',  ( -40.34137639590981195, 32.05937500034139731, 29.30972558990012189 ) ) ;
#2935 = CYLINDRICAL_SURFACE ( 'NONE', #6732, 2.000000000000001776 ) ;
#2936 = ORIENTED_EDGE ( 'NONE', *, *, #3693, .T. ) ;
#2937 = UNCERTAINTY_MEASURE_WITH_UNIT (LENGTH_MEASURE( 1.000000000000000082E-05 ), #15209, 'distance_accuracy_value', 'NONE');
#2938 = CARTESIAN_POINT ( 'NONE',  ( 40.34137639590981905, 26.65937500034139518, 29.30972558990010768 ) ) ;
#2939 = ORIENTED_EDGE ( 'NONE', *, *, #5033, .F. ) ;
#2940 = CARTESIAN_POINT ( 'NONE',  ( 2.500000000000000000, 242.0000000000000284, -49.99999999999999289 ) ) ;
#2941 = CARTESIAN_POINT ( 'NONE',  ( -15.40903463028480580, 44.25937500034140015, 47.42413220539094709 ) ) ;
#2942 = CARTESIAN_POINT ( 'NONE',  ( -2.464234863135557063, 13.31155363843772932, 101.0000000000000000 ) ) ;
#2943 = CARTESIAN_POINT ( 'NONE',  ( 28.70358715772642455, 282.1599167565164521, 9.907174315453913138 ) ) ;
#2944 = CARTESIAN_POINT ( 'NONE',  ( -25.50583519766042429, 284.7842439685843487, 3.511670395308091219 ) ) ;
#2945 = CARTESIAN_POINT ( 'NONE',  ( 15.40903463028482356, 36.52187500034139589, 47.42413220539093999 ) ) ;
#2946 = CARTESIAN_POINT ( 'NONE',  ( -15.40903463028481646, 37.45937500034139589, -47.42413220539093999 ) ) ;
#2947 = CARTESIAN_POINT ( 'NONE',  ( -17.45639740057859868, 21.16801284050013976, 101.0000000000000000 ) ) ;
#2948 = CARTESIAN_POINT ( 'NONE',  ( -3.219174618344376363E-15, 43.50000000000000000, -52.57311121191334990 ) ) ;
#2949 = CARTESIAN_POINT ( 'NONE',  ( 15.40903463028482356, 48.45937500034140299, 47.42413220539093999 ) ) ;
#2950 = CARTESIAN_POINT ( 'NONE',  ( -40.34137639590981195, 46.12187500034139731, 29.30972558990012189 ) ) ;
#2951 = CARTESIAN_POINT ( 'NONE',  ( -40.34137639590981905, 27.72187500034139873, -29.30972558990011478 ) ) ;
#2952 = EDGE_CURVE ( 'NONE', #7138, #5789, #10642, .T. ) ;
#2953 = CARTESIAN_POINT ( 'NONE',  ( 30.81806926056964002, 46.55937500034139020, 42.41743335407646498 ) ) ;
#2954 = ORIENTED_EDGE ( 'NONE', *, *, #14421, .T. ) ;
#2955 = CARTESIAN_POINT ( 'NONE',  ( -15.45084971874737256, 29.38125000068279746, -47.55282581475767500 ) ) ;
#2956 = ORIENTED_EDGE ( 'NONE', *, *, #12706, .T. ) ;
#2957 = EDGE_CURVE ( 'NONE', #10320, #10461, #8738, .T. ) ;
#2958 = DIRECTION ( 'NONE',  ( -0.000000000000000000, -1.000000000000000000, -0.000000000000000000 ) ) ;
#2959 = DIRECTION ( 'NONE',  ( 0.000000000000000000, 0.000000000000000000, -1.000000000000000000 ) ) ;
#2960 = CARTESIAN_POINT ( 'NONE',  ( -48.98979485566356118, 261.9999999999999432, 10.00000000000000178 ) ) ;
#2961 = CARTESIAN_POINT ( 'NONE',  ( -15.40903463028481646, 49.52187500034140299, -47.42413220539093999 ) ) ;
#2962 = CARTESIAN_POINT ( 'NONE',  ( 40.34137639590981905, 26.65937500034139518, 29.30972558990010768 ) ) ;
#2963 = DIRECTION ( 'NONE',  ( 0.000000000000000000, 0.000000000000000000, 1.000000000000000000 ) ) ;
#2964 =( BOUNDED_CURVE ( )  B_SPLINE_CURVE ( 2, ( #7331, #13384, #1907, #11072, #658, #3247, #9746, #8319, #8404, #13473, #2080, #10982, #16045 ),
 .UNSPECIFIED., .F., .T. ) 
 B_SPLINE_CURVE_WITH_KNOTS ( ( 3, 2, 2, 2, 2, 2, 3 ),
 ( 0.5833333333333333703, 0.5866666666666666696, 0.5933333333333333792, 0.5999999999999999778, 0.6066666666666666874, 0.6133333333333332860, 0.6166666666666666963 ),
 .UNSPECIFIED. ) 
 CURVE ( )  GEOMETRIC_REPRESENTATION_ITEM ( )  RATIONAL_B_SPLINE_CURVE ( ( 0.9755282581475768211, 0.9755282581475771542, 1.000000000000000000, 0.9510565162951535312, 1.000000000000000000, 0.9510565162951535312, 1.000000000000000000, 0.9510565162951535312, 1.000000000000000000, 0.9510565162951535312, 1.000000000000000000, 0.9755282581475763770, 0.9755282581475768211 ) ) 
 REPRESENTATION_ITEM ( '' )  );
#2965 = EDGE_CURVE ( 'NONE', #16436, #10385, #9551, .T. ) ;
#2966 = CARTESIAN_POINT ( 'NONE',  ( 15.40903463028481113, 41.32187500034140015, -47.42413220539094709 ) ) ;
#2967 = DIRECTION ( 'NONE',  ( 1.000000000000000000, 0.000000000000000000, 0.000000000000000000 ) ) ;
#2968 = CARTESIAN_POINT ( 'NONE',  ( 40.34137639590981905, 46.72187500034139873, 29.30972558990010768 ) ) ;
#2969 = CARTESIAN_POINT ( 'NONE',  ( -30.90169943749474513, 45.48125000068279178, -42.53254041760200721 ) ) ;
#2970 = ORIENTED_EDGE ( 'NONE', *, *, #10784, .F. ) ;
#2971 = CARTESIAN_POINT ( 'NONE',  ( -3.210462471511496205E-15, 21.35937500034139092, -52.43083105670540789 ) ) ;
#2972 = EDGE_LOOP ( 'NONE', ( #15403, #2205, #1223 ) ) ;
#2973 = CARTESIAN_POINT ( 'NONE',  ( -30.00000000000000711, 282.0000000000000000, 12.50000000000000000 ) ) ;
#2974 = VERTEX_POINT ( 'NONE', #16115 ) ;
#2975 = CARTESIAN_POINT ( 'NONE',  ( 0.000000000000000000, 28.00000000000000355, -10.00000000000000000 ) ) ;
#2976 = FACE_OUTER_BOUND ( 'NONE', #5313, .T. ) ;
#2977 = CARTESIAN_POINT ( 'NONE',  ( 0.000000000000000000, 22.50000000000000000, 102.0000000000000142 ) ) ;
#2978 = CARTESIAN_POINT ( 'NONE',  ( 40.45084971874737079, 25.19999999999999929, -29.38926261462366440 ) ) ;
#2979 = CARTESIAN_POINT ( 'NONE',  ( -15.40903463028480580, 46.25937500034140015, 47.42413220539094709 ) ) ;
#2980 = CYLINDRICAL_SURFACE ( 'NONE', #2744, 50.00000000000000000 ) ;
#2981 = CARTESIAN_POINT ( 'NONE',  ( -0.5000000000000000000, 245.0000000000000284, 49.99999999999999289 ) ) ;
#2982 = EDGE_CURVE ( 'NONE', #6547, #1767, #508, .T. ) ;
#2983 = CARTESIAN_POINT ( 'NONE',  ( 9.297345850538470396E-15, 92.00000000000001421, -1.969248798088869855E-14 ) ) ;
#2984 = SURFACE_STYLE_USAGE ( .BOTH. , #15778 ) ;
#2985 = LINE ( 'NONE', #8054, #7018 ) ;
#2986 = CARTESIAN_POINT ( 'NONE',  ( 40.45084971874737789, 34.58125000068280031, 29.38926261462365375 ) ) ;
#2987 = CARTESIAN_POINT ( 'NONE',  ( 16.79120288457601262, 27.43006142852259899, 101.0000000000000000 ) ) ;
#2988 = VECTOR ( 'NONE', #14774, 1000.000000000000000 ) ;
#2989 = CARTESIAN_POINT ( 'NONE',  ( -1.486087262401750042, 13.10364194761997503, 102.0000000000000142 ) ) ;
#2990 = CARTESIAN_POINT ( 'NONE',  ( -2.500000000000000000, 247.0000000000000284, -44.93050188902856945 ) ) ;
#2991 = ORIENTED_EDGE ( 'NONE', *, *, #294, .T. ) ;
#2992 = CARTESIAN_POINT ( 'NONE',  ( -40.34137639590981905, 35.65937500034139873, -29.30972558990011478 ) ) ;
#2993 = ORIENTED_EDGE ( 'NONE', *, *, #15459, .T. ) ;
#2994 = EDGE_LOOP ( 'NONE', ( #15651, #3835, #7901, #608 ) ) ;
#2995 = FACE_OUTER_BOUND ( 'NONE', #3645, .T. ) ;
#2996 = DIRECTION ( 'NONE',  ( -0.000000000000000000, 1.000000000000000000, -0.000000000000000000 ) ) ;
#2997 = CARTESIAN_POINT ( 'NONE',  ( 15.40903463028482356, 22.45937500034139589, 47.42413220539093999 ) ) ;
#2999 = EDGE_LOOP ( 'NONE', ( #1023, #2877, #14697, #16344 ) ) ;
#2998 = AXIS2_PLACEMENT_3D ( 'NONE', #6852, #13232, #9408 ) ;
#3000 = EDGE_CURVE ( 'NONE', #14186, #6058, #2212, .T. ) ;
#3001 = LINE ( 'NONE', #3242, #10790 ) ;
#3002 = DIRECTION ( 'NONE',  ( 0.000000000000000000, 0.000000000000000000, 1.000000000000000000 ) ) ;
#3003 = CARTESIAN_POINT ( 'NONE',  ( -40.34137639590981905, 25.72187500034139518, -29.30972558990011478 ) ) ;
#3004 = LINE ( 'NONE', #9253, #1502 ) ;
#3005 = CARTESIAN_POINT ( 'NONE',  ( -20.00000000000000355, 307.0000000000000568, -2.499999999999998668 ) ) ;
#3006 = CARTESIAN_POINT ( 'NONE',  ( -48.07045810499274552, 20.00000000000000355, 13.25585611146461140 ) ) ;
#3007 = CARTESIAN_POINT ( 'NONE',  ( 49.86468353125000164, 26.92187500034139802, -6.106662507704105588E-15 ) ) ;
#3008 = CARTESIAN_POINT ( 'NONE',  ( 3.009228475883622522, 5.937825933686468716, 101.6666710451724214 ) ) ;
#3009 = CARTESIAN_POINT ( 'NONE',  ( 30.90169943749475578, 36.70000000000000995, 42.53254041760200010 ) ) ;
#3010 = CARTESIAN_POINT ( 'NONE',  ( -15.40903463028481646, 35.45937500034139589, -47.42413220539093999 ) ) ;
#3011 = AXIS2_PLACEMENT_3D ( 'NONE', #3005, #14221, #6857 ) ;
#3012 = DIRECTION ( 'NONE',  ( -0.000000000000000000, -0.000000000000000000, -1.000000000000000000 ) ) ;
#3013 = ORIENTED_EDGE ( 'NONE', *, *, #8619, .F. ) ;
#3014 = CARTESIAN_POINT ( 'NONE',  ( 49.86468353125000164, 28.85937500034139802, -6.106662507704105588E-15 ) ) ;
#3015 = ORIENTED_EDGE ( 'NONE', *, *, #10406, .T. ) ;
#3016 = DIRECTION ( 'NONE',  ( -0.000000000000000000, -1.000000000000000000, -0.000000000000000000 ) ) ;
#3017 = CARTESIAN_POINT ( 'NONE',  ( 40.34137639590981195, 41.05937500034139731, -29.30972558990011834 ) ) ;
#3018 = CARTESIAN_POINT ( 'NONE',  ( 0.5000000000000000000, 244.0000000000000284, 49.99999999999999289 ) ) ;
#3019 = CARTESIAN_POINT ( 'NONE',  ( 25.75618375337400678, 283.9316295015381115, 8.256183753372502210 ) ) ;
#3020 = AXIS2_PLACEMENT_3D ( 'NONE', #6336, #16384, #15288 ) ;
#3021 = CARTESIAN_POINT ( 'NONE',  ( -27.40717431545314042, 282.1599167565163384, 11.20358715772689528 ) ) ;
#3022 = CARTESIAN_POINT ( 'NONE',  ( 49.86468353124999453, 37.02187500034138878, -16.20201782572376459 ) ) ;
#3023 = CARTESIAN_POINT ( 'NONE',  ( 30.81806926056962936, 39.15937500034139873, -42.41743335407646498 ) ) ;
#3024 = DIRECTION ( 'NONE',  ( 0.9945218953682744001, -0.1045284632676436315, 0.000000000000000000 ) ) ;
#3025 = CARTESIAN_POINT ( 'NONE',  ( 40.45084971874737079, 43.20000000000000284, -29.38926261462366440 ) ) ;
#3026 = CARTESIAN_POINT ( 'NONE',  ( -3.219174618344376363E-15, 23.28125000068279959, -52.57311121191334990 ) ) ;
#3027 = CARTESIAN_POINT ( 'NONE',  ( -40.34137639590981195, 42.12187500034139731, 29.30972558990012189 ) ) ;
#3028 = EDGE_CURVE ( 'NONE', #7197, #2833, #8692, .T. ) ;
#3029 = CARTESIAN_POINT ( 'NONE',  ( 49.86468353125001585, 24.82187500034139305, 16.20201782572375038 ) ) ;
#3030 = EDGE_CURVE ( 'NONE', #16226, #12784, #14768, .T. ) ;
#3031 = VECTOR ( 'NONE', #12851, 1000.000000000000000 ) ;
#3032 = ORIENTED_EDGE ( 'NONE', *, *, #1513, .F. ) ;
#3033 = CARTESIAN_POINT ( 'NONE',  ( -30.90169943749474868, 29.48125000068279888, -42.53254041760200721 ) ) ;
#3034 = ORIENTED_EDGE ( 'NONE', *, *, #9677, .T. ) ;
#3035 = CARTESIAN_POINT ( 'NONE',  ( -43.87482193696061472, 267.0000000000000000, -10.00000000000000178 ) ) ;
#3036 = DIRECTION ( 'NONE',  ( -0.000000000000000000, 1.000000000000000000, -0.000000000000000000 ) ) ;
#3037 = CARTESIAN_POINT ( 'NONE',  ( -40.34137639590981195, 44.12187500034139731, 29.30972558990012189 ) ) ;
#3038 = CARTESIAN_POINT ( 'NONE',  ( 49.86468353124999453, 24.95937500034139234, -16.20201782572376459 ) ) ;
#3039 = EDGE_CURVE ( 'NONE', #8435, #436, #6579, .T. ) ;
#3040 = CONICAL_SURFACE ( 'NONE', #12336, 65.00000000000000000, 0.08726646259971666819 ) ;
#3041 = CARTESIAN_POINT ( 'NONE',  ( 9.227956911499398113E-15, 102.0000000000000142, -9.080892972013931086 ) ) ;
#3042 = CIRCLE ( 'NONE', #12338, 10.00000000000000000 ) ;
#3043 = CARTESIAN_POINT ( 'NONE',  ( -40.34137639590981905, 41.72187500034139873, -29.30972558990011478 ) ) ;
#3044 = CARTESIAN_POINT ( 'NONE',  ( -15.40903463028480580, 44.32187500034140015, 47.42413220539094709 ) ) ;
#3045 = CARTESIAN_POINT ( 'NONE',  ( 15.45084971874736723, 31.39999999999999858, -47.55282581475768211 ) ) ;
#3046 = ORIENTED_EDGE ( 'NONE', *, *, #15738, .F. ) ;
#3047 = CARTESIAN_POINT ( 'NONE',  ( -30.81806926056962226, 42.22187500034139163, 42.41743335407647919 ) ) ;
#3048 = EDGE_LOOP ( 'NONE', ( #4640, #11034, #186, #6569 ) ) ;
#3049 = ORIENTED_EDGE ( 'NONE', *, *, #3118, .T. ) ;
#3050 = CIRCLE ( 'NONE', #9691, 16.50000000000000711 ) ;
#3051 = VECTOR ( 'NONE', #3664, 1000.000000000000000 ) ;
#3052 = EDGE_CURVE ( 'NONE', #3406, #793, #8465, .T. ) ;
#3053 = CARTESIAN_POINT ( 'NONE',  ( 0.000000000000000000, 272.0000000000000000, 0.000000000000000000 ) ) ;
#3054 = CARTESIAN_POINT ( 'NONE',  ( 0.000000000000000000, 45.07596123493892293, 0.000000000000000000 ) ) ;
#3055 =( BOUNDED_CURVE ( )  B_SPLINE_CURVE ( 3, ( #10073, #7734, #1242, #6337 ),
 .UNSPECIFIED., .F., .T. ) 
 B_SPLINE_CURVE_WITH_KNOTS ( ( 4, 4 ),
 ( 4.523772594209285458, 4.901005366560093002 ),
 .UNSPECIFIED. ) 
 CURVE ( )  GEOMETRIC_REPRESENTATION_ITEM ( )  RATIONAL_B_SPLINE_CURVE ( ( 1.000000000000000000, 0.9881764018959044993, 0.9881764018959044993, 1.000000000000000000 ) ) 
 REPRESENTATION_ITEM ( '' )  );
#3056 = CARTESIAN_POINT ( 'NONE',  ( 6.123233995736766085E-15, 193.4213562373095385, 50.00000000000000000 ) ) ;
#3057 = CARTESIAN_POINT ( 'NONE',  ( 30.90169943749475578, 22.69999999999999929, 42.53254041760200010 ) ) ;
#3058 = CARTESIAN_POINT ( 'NONE',  ( 15.40903463028481113, 41.25937500034139305, -47.42413220539094709 ) ) ;
#3059 = CARTESIAN_POINT ( 'NONE',  ( 40.45084971874737789, 48.58125000068280031, 29.38926261462365375 ) ) ;
#3060 = DIRECTION ( 'NONE',  ( -1.000000000000000000, -0.000000000000000000, -0.000000000000000000 ) ) ;
#3061 = FACE_BOUND ( 'NONE', #2390, .T. ) ;
#3062 =( LENGTH_UNIT ( ) NAMED_UNIT ( * ) SI_UNIT ( .MILLI., .METRE. ) );
#3063 = CARTESIAN_POINT ( 'NONE',  ( -10.68655108903816142, 8.641875097208238543, 101.0000000000000000 ) ) ;
#3064 = CARTESIAN_POINT ( 'NONE',  ( -3.219174618344376363E-15, 33.28125000068280315, -52.57311121191334990 ) ) ;
#3065 = DIRECTION ( 'NONE',  ( 0.000000000000000000, 0.000000000000000000, -1.000000000000000000 ) ) ;
#3066 = CIRCLE ( 'NONE', #12357, 90.84711083310548929 ) ;
#3067 = EDGE_CURVE ( 'NONE', #5789, #15481, #12823, .T. ) ;
#3068 = DIRECTION ( 'NONE',  ( 0.000000000000000000, -0.000000000000000000, 1.000000000000000000 ) ) ;
#3069 = AXIS2_PLACEMENT_3D ( 'NONE', #3248, #6004, #16141 ) ;
#3070 = ORIENTED_EDGE ( 'NONE', *, *, #3752, .T. ) ;
#3071 = CARTESIAN_POINT ( 'NONE',  ( 9.631387414534489405E-15, 34.35937500034139447, 52.43083105670540789 ) ) ;
#3072 = EDGE_LOOP ( 'NONE', ( #5934, #6574, #10932, #11783 ) ) ;
#3073 = ORIENTED_EDGE ( 'NONE', *, *, #6682, .F. ) ;
#3074 = CARTESIAN_POINT ( 'NONE',  ( 50.00000000000000000, 48.78125000068279604, -6.123233995736766085E-15 ) ) ;
#3075 = CIRCLE ( 'NONE', #14475, 4.000000000000001776 ) ;
#3076 = VECTOR ( 'NONE', #2530, 1000.000000000000000 ) ;
#3077 = CIRCLE ( 'NONE', #14231, 5.000000000000000888 ) ;
#3078 = DIRECTION ( 'NONE',  ( 5.069245582283711292E-17, 1.000000000000000000, -8.780190904559502465E-17 ) ) ;
#3079 = CARTESIAN_POINT ( 'NONE',  ( -40.34137639590981905, 25.65937500034139518, -29.30972558990011478 ) ) ;
#3080 = AXIS2_PLACEMENT_3D ( 'NONE', #6923, #3002, #15795 ) ;
#3081 = ORIENTED_EDGE ( 'NONE', *, *, #9637, .T. ) ;
#3082 = PRODUCT_DEFINITION_SHAPE ( 'NONE', 'NONE',  #5699 ) ;
#3083 = DIRECTION ( 'NONE',  ( -0.9135454576426005335, -0.4067366430758011520, 0.000000000000000000 ) ) ;
#3084 = CARTESIAN_POINT ( 'NONE',  ( 7.919222016226693306, 22.55125428154684286, 50.00000000000003553 ) ) ;
#3085 = CARTESIAN_POINT ( 'NONE',  ( 7.394441145214595501, 28.48516834767053751, 102.0000000000000142 ) ) ;
#3086 = CARTESIAN_POINT ( 'NONE',  ( 48.35726954556789536, 24.99999999999999645, -12.16803787670825265 ) ) ;
#3087 = CARTESIAN_POINT ( 'NONE',  ( -30.90169943749473447, 38.08125000068280031, 42.53254041760200721 ) ) ;
#3088 = CARTESIAN_POINT ( 'NONE',  ( 14.90054083259177453, 13.30529623682518370, 96.51097829310403142 ) ) ;
#3089 = CARTESIAN_POINT ( 'NONE',  ( -47.07787634996812187, 19.99999999999999645, 16.43739640347152786 ) ) ;
#3090 = EDGE_CURVE ( 'NONE', #6101, #7762, #6471, .T. ) ;
#3091 = CARTESIAN_POINT ( 'NONE',  ( -3.210462471511496205E-15, 25.42187500034139447, -52.43083105670540789 ) ) ;
#3092 = CARTESIAN_POINT ( 'NONE',  ( -7.919222016226934890, 22.44874571845315714, 49.99999999999996447 ) ) ;
#3093 = EDGE_CURVE ( 'NONE', #9838, #13826, #12732, .T. ) ;
#3094 = AXIS2_PLACEMENT_3D ( 'NONE', #1520, #9414, #2759 ) ;
#3095 = CARTESIAN_POINT ( 'NONE',  ( 50.00000000000000711, 32.89999999999999147, 16.24598481164530739 ) ) ;
#3096 = CARTESIAN_POINT ( 'NONE',  ( 30.81806926056964002, 24.55937500034139376, 42.41743335407647209 ) ) ;
#3097 = AXIS2_PLACEMENT_3D ( 'NONE', #10227, #3826, #2573 ) ;
#3098 = CONICAL_SURFACE ( 'NONE', #6550, 16.50000000000000711, 0.7853981633974447263 ) ;
#3099 = FACE_OUTER_BOUND ( 'NONE', #6152, .T. ) ;
#3100 = ORIENTED_EDGE ( 'NONE', *, *, #6422, .F. ) ;
#3101 = CARTESIAN_POINT ( 'NONE',  ( 49.86468353124999453, 32.95937500034138878, -16.20201782572376104 ) ) ;
#3102 = ORIENTED_EDGE ( 'NONE', *, *, #5714, .F. ) ;
#3103 = DIRECTION ( 'NONE',  ( 1.000000000000000000, 0.000000000000000000, -0.000000000000000000 ) ) ;
#3104 = CARTESIAN_POINT ( 'NONE',  ( 30.81806926056964002, 42.55937500034139020, 42.41743335407647209 ) ) ;
#3105 = AXIS2_PLACEMENT_3D ( 'NONE', #8647, #6413, #4852 ) ;
#3106 = CARTESIAN_POINT ( 'NONE',  ( 27.61612561545807409, 282.5087415087664908, 10.11612561546265354 ) ) ;
#3107 = EDGE_CURVE ( 'NONE', #3799, #1042, #12368, .T. ) ;
#3108 = AXIS2_PLACEMENT_3D ( 'NONE', #15384, #10159, #8234 ) ;
#3109 = CARTESIAN_POINT ( 'NONE',  ( -20.06446087899944786, 286.3455096218657445, 7.532230439500318120 ) ) ;
#3110 = EDGE_CURVE ( 'NONE', #9620, #10200, #6470, .T. ) ;
#3111 = CARTESIAN_POINT ( 'NONE',  ( -30.81806926056963292, 29.62187500034139376, -42.41743335407647209 ) ) ;
#3112 = CARTESIAN_POINT ( 'NONE',  ( -40.34137639590981905, 35.65937500034139873, -29.30972558990011478 ) ) ;
#3113 = CARTESIAN_POINT ( 'NONE',  ( -7.919222016226816763, 43.55125428154684641, -49.99999999999999289 ) ) ;
#3114 = CARTESIAN_POINT ( 'NONE',  ( 40.34137639590981195, 31.12187500034139731, -29.30972558990011834 ) ) ;
#3115 = CARTESIAN_POINT ( 'NONE',  ( -40.45084971874737079, 44.20000000000000284, 29.38926261462367151 ) ) ;
#3116 = CARTESIAN_POINT ( 'NONE',  ( 30.90169943749474157, 21.08125000068279675, -42.53254041760200721 ) ) ;
#3117 = CARTESIAN_POINT ( 'NONE',  ( 15.40903463028482356, 44.52187500034139589, 47.42413220539093999 ) ) ;
#3118 = EDGE_CURVE ( 'NONE', #12043, #12621, #13851, .T. ) ;
#3119 = CARTESIAN_POINT ( 'NONE',  ( -49.86468353125000164, 21.92187500034139802, 0.000000000000000000 ) ) ;
#3120 = VECTOR ( 'NONE', #3176, 1000.000000000000114 ) ;
#3121 = EDGE_LOOP ( 'NONE', ( #4200, #5539, #1333, #14827 ) ) ;
#3122 = CARTESIAN_POINT ( 'NONE',  ( -30.81806926056963292, 47.55937500034139731, -42.41743335407646498 ) ) ;
#3123 = ORIENTED_EDGE ( 'NONE', *, *, #8180, .T. ) ;
#3124 = CARTESIAN_POINT ( 'NONE',  ( -15.45084971874736368, 32.18125000068279462, 47.55282581475768211 ) ) ;
#3125 = EDGE_LOOP ( 'NONE', ( #1944, #433, #2585, #2401, #5991, #9150, #14028, #165, #364, #739, #12218, #8005, #8901, #4818, #16174, #15515, #8971, #325, #10770, #8458, #16106, #12092, #10381, #6476, #14558, #12111, #12135, #5466, #11130, #1660, #11018, #1433, #5804, #1041, #11389, #1636, #7841, #12788, #15811, #3454, #7824, #7645, #10289, #15362, #2377, #14337, #13823, #5145, #11457, #9756, #7319, #2993, #8149, #13317, #5823, #57, #12022, #12258, #13334, #5657, #12176 ) ) ;
#3126 = CARTESIAN_POINT ( 'NONE',  ( -20.00000000000000355, 307.0000000000000568, -2.499999999999998668 ) ) ;
#3127 = DIRECTION ( 'NONE',  ( -0.9135454576426059736, 0.4067366430757887730, 0.000000000000000000 ) ) ;
#3128 = CARTESIAN_POINT ( 'NONE',  ( -15.40903463028480580, 38.32187500034140015, 47.42413220539094709 ) ) ;
#3129 = CARTESIAN_POINT ( 'NONE',  ( 40.34137639590981195, 23.05937500034139731, -29.30972558990011834 ) ) ;
#3130 = CARTESIAN_POINT ( 'NONE',  ( 0.000000000000000000, 52.00000000000000711, 0.000000000000000000 ) ) ;
#3131 = ITEM_DEFINED_TRANSFORMATION ( 'NONE', 'NONE', #16091,  #15812 ) ;
#3132 = CARTESIAN_POINT ( 'NONE',  ( 9.657523855033129090E-15, 38.50000000000000711, 52.57311121191334990 ) ) ;
#3133 = CARTESIAN_POINT ( 'NONE',  ( 40.34137639590981195, 49.12187500034139731, -29.30972558990011834 ) ) ;
#3134 = DIRECTION ( 'NONE',  ( 0.000000000000000000, -1.000000000000000000, 0.000000000000000000 ) ) ;
#3135 = ORIENTED_EDGE ( 'NONE', *, *, #1334, .F. ) ;
#3136 = CARTESIAN_POINT ( 'NONE',  ( -49.86468353124999453, 42.02187500034139589, 16.20201782572377525 ) ) ;
#3137 = EDGE_LOOP ( 'NONE', ( #3032, #5277, #14535, #2645 ) ) ;
#3138 = ORIENTED_EDGE ( 'NONE', *, *, #5655, .T. ) ;
#3139 = LINE ( 'NONE', #2975, #15053 ) ;
#3140 = LINE ( 'NONE', #7970, #6262 ) ;
#3141 = DIRECTION ( 'NONE',  ( -0.000000000000000000, -1.000000000000000000, -0.000000000000000000 ) ) ;
#3142 = DIRECTION ( 'NONE',  ( -0.8660254037844433705, 0.4999999999999918399, 0.000000000000000000 ) ) ;
#3143 = CARTESIAN_POINT ( 'NONE',  ( -30.81806926056962226, 46.15937500034139873, 42.41743335407647919 ) ) ;
#3144 = CARTESIAN_POINT ( 'NONE',  ( 6.123233995736766085E-15, 20.00000000000000355, -50.00000000000000000 ) ) ;
#3145 = LINE ( 'NONE', #8219, #6902 ) ;
#3146 = CARTESIAN_POINT ( 'NONE',  ( 1.075479105333760460E-14, 274.0000000000000000, -87.81953344283027718 ) ) ;
#3147 =( NAMED_UNIT ( * ) PLANE_ANGLE_UNIT ( ) SI_UNIT ( $, .RADIAN. ) );
#3148 = LINE ( 'NONE', #3226, #5441 ) ;
#3149 = FACE_BOUND ( 'NONE', #5769, .T. ) ;
#3150 = EDGE_CURVE ( 'NONE', #4234, #12110, #14835, .T. ) ;
#3151 = DIRECTION ( 'NONE',  ( 0.9961946980917455452, -0.08715574274765797158, 0.000000000000000000 ) ) ;
#3152 = CARTESIAN_POINT ( 'NONE',  ( -7.436122194756538129, 37.97250723688134855, 101.3333374614808662 ) ) ;
#3153 = VERTEX_POINT ( 'NONE', #1213 ) ;
#3154 = CARTESIAN_POINT ( 'NONE',  ( 49.86468353124999453, 28.95937500034139944, -16.20201782572376459 ) ) ;
#3155 = ORIENTED_EDGE ( 'NONE', *, *, #4858, .T. ) ;
#3156 = VERTEX_POINT ( 'NONE', #12779 ) ;
#3157 = VERTEX_POINT ( 'NONE', #2305 ) ;
#3159 = EDGE_CURVE ( 'NONE', #7881, #2646, #1380, .T. ) ;
#3158 =( BOUNDED_CURVE ( )  B_SPLINE_CURVE ( 2, ( #9624, #14928, #8703, #1124, #880, #6219, #8461 ),
 .UNSPECIFIED., .F., .F. ) 
 B_SPLINE_CURVE_WITH_KNOTS ( ( 3, 2, 2, 3 ),
 ( 0.000000000000000000, 0.006666666666666667095, 0.01333333333333333419, 0.01666666666666666990 ),
 .UNSPECIFIED. ) 
 CURVE ( )  GEOMETRIC_REPRESENTATION_ITEM ( )  RATIONAL_B_SPLINE_CURVE ( ( 1.000000000000000000, 0.9510565162951535312, 1.000000000000000000, 0.9510565162951535312, 1.000000000000000000, 0.9755282581475768211, 0.9755282581475768211 ) ) 
 REPRESENTATION_ITEM ( '' )  );
#3160 = ADVANCED_FACE ( 'NONE', ( #126 ), #12994, .T. ) ;
#3161 = MANIFOLD_SOLID_BREP ( 'Cavity1', #12370 ) ;
#3162 = CARTESIAN_POINT ( 'NONE',  ( -15.45084971874737256, 47.38125000068279746, -47.55282581475767500 ) ) ;
#3163 = AXIS2_PLACEMENT_3D ( 'NONE', #12305, #1072, #6001 ) ;
#3164 = FACE_OUTER_BOUND ( 'NONE', #14409, .T. ) ;
#3165 = CARTESIAN_POINT ( 'NONE',  ( -15.40903463028480580, 24.25937500034139660, 47.42413220539094709 ) ) ;
#3166 = ORIENTED_EDGE ( 'NONE', *, *, #8349, .T. ) ;
#3167 = EDGE_CURVE ( 'NONE', #842, #13696, #15350, .T. ) ;
#3168 = CARTESIAN_POINT ( 'NONE',  ( 2.978552182361884590E-14, 47.50000000000000711, -50.00000000000000000 ) ) ;
#3169 = CARTESIAN_POINT ( 'NONE',  ( 6.000000000000001776, 22.50000000000000000, 101.0000000000000000 ) ) ;
#3170 = DIRECTION ( 'NONE',  ( -0.000000000000000000, 1.000000000000000000, -0.000000000000000000 ) ) ;
#3171 = CARTESIAN_POINT ( 'NONE',  ( 49.86468353125000164, 28.92187500034139802, -6.106662507704105588E-15 ) ) ;
#3172 = ADVANCED_FACE ( 'NONE', ( #15260 ), #3969, .F. ) ;
#3173 = CARTESIAN_POINT ( 'NONE',  ( 17.50000000000000355, 21.92738356273111222, 94.52735820379716358 ) ) ;
#3174 = CARTESIAN_POINT ( 'NONE',  ( -47.44954343046507717, 20.00000000000001066, 15.33151233206156228 ) ) ;
#3175 = CARTESIAN_POINT ( 'NONE',  ( 49.86468353125001585, 22.82187500034139305, 16.20201782572375038 ) ) ;
#3176 = DIRECTION ( 'NONE',  ( 0.000000000000000000, 0.7890408728378107694, 0.6143407043256581268 ) ) ;
#3177 = CARTESIAN_POINT ( 'NONE',  ( 30.90169943749474157, 33.30000000000000426, -42.53254041760200721 ) ) ;
#3178 = CARTESIAN_POINT ( 'NONE',  ( 40.34137639590981195, 25.05937500034139376, -29.30972558990011834 ) ) ;
#3179 = CARTESIAN_POINT ( 'NONE',  ( -15.40903463028481646, 47.45937500034139589, -47.42413220539093999 ) ) ;
#3180 = ORIENTED_EDGE ( 'NONE', *, *, #12207, .T. ) ;
#3181 = CARTESIAN_POINT ( 'NONE',  ( 49.86468353125000164, 30.85937500034139802, -6.106662507704105588E-15 ) ) ;
#3182 = VERTEX_POINT ( 'NONE', #7393 ) ;
#3183 = CYLINDRICAL_SURFACE ( 'NONE', #4705, 2.000000000000001776 ) ;
#3184 = CARTESIAN_POINT ( 'NONE',  ( 40.34137639590981905, 40.65937500034139873, 29.30972558990010768 ) ) ;
#3185 = DIRECTION ( 'NONE',  ( 0.000000000000000000, 1.000000000000000000, 0.000000000000000000 ) ) ;
#3186 = CARTESIAN_POINT ( 'NONE',  ( 7.919222016226791006, 44.33250428222964246, 50.00000000000000711 ) ) ;
#3187 = MANIFOLD_SOLID_BREP ( 'Cut-Extrude1', #7606 ) ;
#3188 = CARTESIAN_POINT ( 'NONE',  ( 30.81806926056962936, 27.22187500034139518, -42.41743335407647209 ) ) ;
#3189 = CARTESIAN_POINT ( 'NONE',  ( 15.40903463028482356, 36.45937500034139589, 47.42413220539093999 ) ) ;
#3190 = FACE_OUTER_BOUND ( 'NONE', #15995, .T. ) ;
#3191 = CARTESIAN_POINT ( 'NONE',  ( -49.86468353124999453, 32.02187500034139589, 16.20201782572377525 ) ) ;
#3192 = CARTESIAN_POINT ( 'NONE',  ( 40.45084971874737789, 38.80000000000000426, 29.38926261462365375 ) ) ;
#3193 = CARTESIAN_POINT ( 'NONE',  ( 15.40903463028482356, 42.45937500034140299, 47.42413220539093999 ) ) ;
#3194 = CARTESIAN_POINT ( 'NONE',  ( -30.81806926056963292, 41.62187500034139020, -42.41743335407647209 ) ) ;
#3195 = CARTESIAN_POINT ( 'NONE',  ( -40.45084971874737789, 49.80000000000000426, -29.38926261462365730 ) ) ;
#3196 = ORIENTED_EDGE ( 'NONE', *, *, #10399, .F. ) ;
#3197 = CARTESIAN_POINT ( 'NONE',  ( -15.83973438765502451, 27.12091057352761325, 102.0000000000000142 ) ) ;
#3198 = ORIENTED_EDGE ( 'NONE', *, *, #6749, .T. ) ;
#3199 = ORIENTED_EDGE ( 'NONE', *, *, #3603, .F. ) ;
#3200 = CARTESIAN_POINT ( 'NONE',  ( 15.45084971874736723, 33.18125000068279462, -47.55282581475768211 ) ) ;
#3201 = VERTEX_POINT ( 'NONE', #3889 ) ;
#3202 =( BOUNDED_CURVE ( )  B_SPLINE_CURVE ( 2, ( #12058, #7915, #1673, #9411, #8166, #13235, #1833, #6927, #16218, #10983, #2240, #10904, #10827 ),
 .UNSPECIFIED., .F., .F. ) 
 B_SPLINE_CURVE_WITH_KNOTS ( ( 3, 2, 2, 2, 2, 2, 3 ),
 ( 0.08333333333333334259, 0.08666666666666666963, 0.09333333333333333759, 0.1000000000000000056, 0.1066666666666666735, 0.1133333333333333276, 0.1166666666666666685 ),
 .UNSPECIFIED. ) 
 CURVE ( )  GEOMETRIC_REPRESENTATION_ITEM ( )  RATIONAL_B_SPLINE_CURVE ( ( 0.9755282581475768211, 0.9755282581475768211, 1.000000000000000000, 0.9510565162951535312, 1.000000000000000000, 0.9510565162951535312, 1.000000000000000000, 0.9510565162951535312, 1.000000000000000000, 0.9510565162951535312, 1.000000000000000000, 0.9755282581475767101, 0.9755282581475768211 ) ) 
 REPRESENTATION_ITEM ( '' )  );
#3203 = DIRECTION ( 'NONE',  ( 0.000000000000000000, 1.000000000000000000, 0.000000000000000000 ) ) ;
#3204 = CARTESIAN_POINT ( 'NONE',  ( -30.81806926056962226, 42.22187500034139163, 42.41743335407647209 ) ) ;
#3205 = ADVANCED_FACE ( 'NONE', ( #10373 ), #218, .T. ) ;
#3206 = CARTESIAN_POINT ( 'NONE',  ( 49.86468353125000164, 46.92187500034139447, -6.106662507704105588E-15 ) ) ;
#3207 = DIRECTION ( 'NONE',  ( 0.000000000000000000, 0.000000000000000000, -1.000000000000000000 ) ) ;
#3208 = CONTEXT_DEPENDENT_SHAPE_REPRESENTATION ( #10364, #9459 ) ;
#3209 = CARTESIAN_POINT ( 'NONE',  ( -15.45084971874737256, 35.60000000000000142, -47.55282581475767500 ) ) ;
#3210 = B_SPLINE_CURVE_WITH_KNOTS ( 'NONE', 3,
 ( #682, #4117, #7937, #6791 ),
 .UNSPECIFIED., .F., .F.,
 ( 4, 4 ),
 ( 2.829004760666361398E-07, 0.001414802801989365486 ),
 .UNSPECIFIED. ) ;
#3211 = CARTESIAN_POINT ( 'NONE',  ( 40.34137639590981905, 38.72187500034139873, 29.30972558990010768 ) ) ;
#3212 = CARTESIAN_POINT ( 'NONE',  ( -49.99999999999999289, 45.68125000068280173, -16.24598481164531449 ) ) ;
#3213 = ORIENTED_EDGE ( 'NONE', *, *, #8420, .T. ) ;
#3214 = CARTESIAN_POINT ( 'NONE',  ( -49.86468353124999453, 40.02187500034140299, 16.20201782572377525 ) ) ;
#3215 = ORIENTED_EDGE ( 'NONE', *, *, #6051, .T. ) ;
#3216 = ORIENTED_EDGE ( 'NONE', *, *, #15742, .T. ) ;
#3217 = EDGE_LOOP ( 'NONE', ( #4738, #5370, #12298, #6596 ) ) ;
#3218 = FACE_OUTER_BOUND ( 'NONE', #10834, .T. ) ;
#3219 = CARTESIAN_POINT ( 'NONE',  ( 8.660254037844387298, 20.00000000000000355, 5.000000000000000000 ) ) ;
#3220 = LINE ( 'NONE', #13119, #519 ) ;
#3221 = CARTESIAN_POINT ( 'NONE',  ( 15.45084971874737789, 36.38125000068279746, 47.55282581475767500 ) ) ;
#3222 = CARTESIAN_POINT ( 'NONE',  ( -49.86468353124999453, 37.75937500034140015, -16.20201782572375393 ) ) ;
#3223 = CARTESIAN_POINT ( 'NONE',  ( 9.631387414534489405E-15, 46.35937500034139447, 52.43083105670540789 ) ) ;
#3224 = CARTESIAN_POINT ( 'NONE',  ( 15.45084971874736723, 25.40000000000000213, -47.55282581475768211 ) ) ;
#3225 = CARTESIAN_POINT ( 'NONE',  ( -49.86468353125000164, 19.92187500034139447, 0.000000000000000000 ) ) ;
#3226 = CARTESIAN_POINT ( 'NONE',  ( -9.500222237632405253, 22.00424054664139817, 101.0000000000000000 ) ) ;
#3227 = CARTESIAN_POINT ( 'NONE',  ( -15.45084971874737256, 45.60000000000000142, -47.55282581475767500 ) ) ;
#3228 = LINE ( 'NONE', #2140, #8970 ) ;
#3229 = CARTESIAN_POINT ( 'NONE',  ( -6.725310538855818976, 29.22831317314782851, 102.0000000000000142 ) ) ;
#3230 = ORIENTED_EDGE ( 'NONE', *, *, #16166, .T. ) ;
#3231 = ADVANCED_BREP_SHAPE_REPRESENTATION ( '', ( #8848, #15812 ), #1480 ) ;
#3232 = EDGE_CURVE ( 'NONE', #12675, #5661, #1466, .T. ) ;
#3233 = CARTESIAN_POINT ( 'NONE',  ( 15.40903463028482356, 28.45937500034139589, 47.42413220539093999 ) ) ;
#3234 = VERTEX_POINT ( 'NONE', #11620 ) ;
#3235 = ORIENTED_EDGE ( 'NONE', *, *, #11996, .F. ) ;
#3236 = ORIENTED_EDGE ( 'NONE', *, *, #6952, .F. ) ;
#3237 = CARTESIAN_POINT ( 'NONE',  ( 15.45084971874737789, 42.38125000068279746, 47.55282581475767500 ) ) ;
#3238 = DIRECTION ( 'NONE',  ( 6.938893903907231459E-18, -1.000000000000000000, -5.551115123125782702E-17 ) ) ;
#3239 = DIRECTION ( 'NONE',  ( 1.000000000000000000, 0.000000000000000000, 0.000000000000000000 ) ) ;
#3240 = ORIENTED_EDGE ( 'NONE', *, *, #6712, .F. ) ;
#3241 = CARTESIAN_POINT ( 'NONE',  ( -7.919222016226870942, 38.44874571845316069, 49.99999999999997158 ) ) ;
#3242 = CARTESIAN_POINT ( 'NONE',  ( -12.67046914267499069, 34.58135802401869086, 101.0000000000000000 ) ) ;
#3243 = DIRECTION ( 'NONE',  ( 0.3535533905932672916, 0.7071067811865486830, -0.6123724356957968018 ) ) ;
#3244 = APPLICATION_CONTEXT ( 'automotive_design' ) ;
#3245 = CARTESIAN_POINT ( 'NONE',  ( 0.000000000000000000, 267.0000000000000000, 0.000000000000000000 ) ) ;
#3246 = LINE ( 'NONE', #9650, #14287 ) ;
#3247 = CARTESIAN_POINT ( 'NONE',  ( -49.99999999999999289, 32.10000000000000142, 16.24598481164533226 ) ) ;
#3248 = CARTESIAN_POINT ( 'NONE',  ( 0.000000000000000000, 262.0000000000000000, 0.000000000000000000 ) ) ;
#3249 = EDGE_CURVE ( 'NONE', #13278, #11303, #15430, .T. ) ;
#3250 = PRODUCT_RELATED_PRODUCT_CATEGORY ( 'part', '', ( #4148 ) ) ;
#3251 = DIRECTION ( 'NONE',  ( 0.000000000000000000, 0.000000000000000000, 1.000000000000000000 ) ) ;
#3252 = CARTESIAN_POINT ( 'NONE',  ( -46.00570371104000600, 20.06239642599078365, 21.51344788172391631 ) ) ;
#3253 = CYLINDRICAL_SURFACE ( 'NONE', #7628, 50.00000000000000000 ) ;
#3254 = CARTESIAN_POINT ( 'NONE',  ( 40.45084971874737789, 36.79999999999999716, 29.38926261462365375 ) ) ;
#3255 = CARTESIAN_POINT ( 'NONE',  ( -15.40903463028481646, 27.45937500034139944, -47.42413220539093999 ) ) ;
#3256 = CARTESIAN_POINT ( 'NONE',  ( -3.210462471511496205E-15, 47.35937500034138736, -52.43083105670540789 ) ) ;
#3257 = ORIENTED_EDGE ( 'NONE', *, *, #534, .T. ) ;
#3258 = VECTOR ( 'NONE', #5156, 1000.000000000000000 ) ;
#3259 = UNCERTAINTY_MEASURE_WITH_UNIT (LENGTH_MEASURE( 1.000000000000000082E-05 ), #12888, 'distance_accuracy_value', 'NONE');
#3260 = PLANE ( 'NONE',  #5986 ) ;
#3261 = ORIENTED_EDGE ( 'NONE', *, *, #16032, .T. ) ;
#3262 = DIRECTION ( 'NONE',  ( -0.000000000000000000, 1.000000000000000000, -0.000000000000000000 ) ) ;
#3263 = CARTESIAN_POINT ( 'NONE',  ( 15.40903463028482356, 44.45937500034139589, 47.42413220539093999 ) ) ;
#3264 = EDGE_CURVE ( 'NONE', #5374, #758, #10897, .T. ) ;
#3265 = B_SPLINE_CURVE_WITH_KNOTS ( 'NONE', 3,
 ( #6465, #15344, #2629, #5070 ),
 .UNSPECIFIED., .F., .F.,
 ( 4, 4 ),
 ( 2.829004760702349710E-07, 0.001414802801989371557 ),
 .UNSPECIFIED. ) ;
#3266 = CARTESIAN_POINT ( 'NONE',  ( 24.99999999999999645, 312.0000000000000568, 7.500000000000002665 ) ) ;
#3267 = LINE ( 'NONE', #8335, #5665 ) ;
#3268 = CARTESIAN_POINT ( 'NONE',  ( -25.00000000000000711, 287.0000000000000568, 2.500000000000002220 ) ) ;
#3269 = CARTESIAN_POINT ( 'NONE',  ( 40.34137639590981905, 28.72187500034139873, 29.30972558990010768 ) ) ;
#3270 = CARTESIAN_POINT ( 'NONE',  ( -49.86468353124999453, 31.75937500034140015, -16.20201782572375393 ) ) ;
#3271 = CARTESIAN_POINT ( 'NONE',  ( 8.446640517145639571E-15, 26.28125000068279959, 50.00000000000000000 ) ) ;
#3272 = CARTESIAN_POINT ( 'NONE',  ( 49.86468353124999453, 31.02187500034139234, -16.20201782572376459 ) ) ;
#3273 = DIRECTION ( 'NONE',  ( 0.1984322509960792513, 0.9259215214979028552, -0.3213938048432757877 ) ) ;
#3274 = AXIS2_PLACEMENT_3D ( 'NONE', #13919, #3012, #5534 ) ;
#3275 = CARTESIAN_POINT ( 'NONE',  ( -49.86468353124999453, 41.95937500034138878, 16.20201782572377525 ) ) ;
#3276 = CARTESIAN_POINT ( 'NONE',  ( 49.86468353124999453, 37.02187500034138878, -16.20201782572376459 ) ) ;
#3277 = ADVANCED_FACE ( 'NONE', ( #9899 ), #12224, .F. ) ;
#3278 = CARTESIAN_POINT ( 'NONE',  ( 9.631387414534489405E-15, 24.42187500034139447, 52.43083105670540789 ) ) ;
#3279 = ORIENTED_EDGE ( 'NONE', *, *, #4297, .T. ) ;
#3280 = CARTESIAN_POINT ( 'NONE',  ( -30.81806926056962226, 40.15937500034139163, 42.41743335407647209 ) ) ;
#3281 = ORIENTED_EDGE ( 'NONE', *, *, #7386, .F. ) ;
#3282 = CARTESIAN_POINT ( 'NONE',  ( -40.45084971874737789, 31.58125000068280031, -29.38926261462365730 ) ) ;
#3283 = AXIS2_PLACEMENT_3D ( 'NONE', #5171, #7564, #11469 ) ;
#3284 = ORIENTED_EDGE ( 'NONE', *, *, #7560, .T. ) ;
#3285 = CARTESIAN_POINT ( 'NONE',  ( 0.000000000000000000, 20.00000000000000355, 0.000000000000000000 ) ) ;
#3286 = CARTESIAN_POINT ( 'NONE',  ( 49.86468353125001585, 40.82187500034140726, 16.20201782572375038 ) ) ;
#3287 = CARTESIAN_POINT ( 'NONE',  ( 30.81806926056964002, 48.62187500034139731, 42.41743335407647209 ) ) ;
#3288 = DIRECTION ( 'NONE',  ( -0.000000000000000000, 1.000000000000000000, 0.000000000000000000 ) ) ;
#3289 = CARTESIAN_POINT ( 'NONE',  ( -49.86468353124999453, 26.02187500034139944, 16.20201782572377525 ) ) ;
#3290 = CARTESIAN_POINT ( 'NONE',  ( -30.90169943749474868, 39.70000000000000284, -42.53254041760200721 ) ) ;
#3291 = ADVANCED_FACE ( 'NONE', ( #12143 ), #13259, .T. ) ;
#3292 = AXIS2_PLACEMENT_3D ( 'NONE', #10396, #5417, #15533 ) ;
#3293 = CARTESIAN_POINT ( 'NONE',  ( 49.86468353125000164, 40.92187500034139447, -6.106662507704105588E-15 ) ) ;
#3294 = CARTESIAN_POINT ( 'NONE',  ( 1.034642314881058238E-14, 101.0808929720139417, 9.080892972013893782 ) ) ;
#3295 = EDGE_LOOP ( 'NONE', ( #12567, #487, #8570, #11224, #650, #2687, #2497, #6321, #3385, #5557, #13862, #8997 ) ) ;
#3296 = CARTESIAN_POINT ( 'NONE',  ( 15.40903463028482356, 44.52187500034139589, 47.42413220539093999 ) ) ;
#3297 = ORIENTED_EDGE ( 'NONE', *, *, #9014, .F. ) ;
#3298 = ORIENTED_EDGE ( 'NONE', *, *, #14234, .F. ) ;
#3299 =( BOUNDED_CURVE ( )  B_SPLINE_CURVE ( 2, ( #13870, #14039, #2406, #6490, #11546, #4846, #2326, #7410, #6162, #1238, #12552, #15121, #16461 ),
 .UNSPECIFIED., .F., .F. ) 
 B_SPLINE_CURVE_WITH_KNOTS ( ( 3, 2, 2, 2, 2, 2, 3 ),
 ( 0.7500000000000000000, 0.7533333333333332993, 0.7600000000000000089, 0.7666666666666667185, 0.7733333333333333171, 0.7800000000000000266, 0.7833333333333333259 ),
 .UNSPECIFIED. ) 
 CURVE ( )  GEOMETRIC_REPRESENTATION_ITEM ( )  RATIONAL_B_SPLINE_CURVE ( ( 0.9755282581475768211, 0.9755282581475768211, 1.000000000000000000, 0.9510565162951535312, 1.000000000000000000, 0.9510565162951535312, 1.000000000000000000, 0.9510565162951535312, 1.000000000000000000, 0.9510565162951535312, 1.000000000000000000, 0.9755282581475768211, 0.9755282581475768211 ) ) 
 REPRESENTATION_ITEM ( '' )  );
#3300 = ORIENTED_EDGE ( 'NONE', *, *, #12976, .T. ) ;
#3301 = CARTESIAN_POINT ( 'NONE',  ( 0.000000000000000000, 273.6527036446661896, 0.000000000000000000 ) ) ;
#3302 = LINE ( 'NONE', #6062, #13938 ) ;
#3303 = AXIS2_PLACEMENT_3D ( 'NONE', #2387, #11295, #16355 ) ;
#3304 = CARTESIAN_POINT ( 'NONE',  ( 49.99999999999999289, 27.10000000000000142, -16.24598481164532160 ) ) ;
#3305 = FACE_OUTER_BOUND ( 'NONE', #14373, .T. ) ;
#3306 = CARTESIAN_POINT ( 'NONE',  ( 40.34137639590981195, 35.05937500034139731, -29.30972558990011834 ) ) ;
#3307 = DIRECTION ( 'NONE',  ( 0.000000000000000000, 1.541976423090494894E-16, 1.000000000000000000 ) ) ;
#3308 = CARTESIAN_POINT ( 'NONE',  ( -7.919222016226934890, 30.44874571845316069, 49.99999999999996447 ) ) ;
#3309 = DIRECTION ( 'NONE',  ( -0.000000000000000000, 1.000000000000000000, -0.000000000000000000 ) ) ;
#3310 = CARTESIAN_POINT ( 'NONE',  ( -2.547328955960238000E-13, 34.28125000068279604, 49.99999999999999289 ) ) ;
#3311 = CARTESIAN_POINT ( 'NONE',  ( 0.000000000000000000, 50.00000000000000000, 0.000000000000000000 ) ) ;
#3312 = CARTESIAN_POINT ( 'NONE',  ( 40.45084971874737789, 42.58125000068280031, 29.38926261462365375 ) ) ;
#3313 = CARTESIAN_POINT ( 'NONE',  ( 0.000000000000000000, 22.50000000000000000, 102.0000000000000142 ) ) ;
#3314 = ORIENTED_EDGE ( 'NONE', *, *, #9141, .F. ) ;
#3315 = AXIS2_PLACEMENT_3D ( 'NONE', #10769, #13179, #10615 ) ;
#3316 = CARTESIAN_POINT ( 'NONE',  ( -30.81806926056962226, 30.15937500034139163, 42.41743335407647919 ) ) ;
#3317 = ORIENTED_EDGE ( 'NONE', *, *, #6451, .T. ) ;
#3318 = VERTEX_POINT ( 'NONE', #11155 ) ;
#3319 = ORIENTED_EDGE ( 'NONE', *, *, #8755, .T. ) ;
#3320 = MANIFOLD_SOLID_BREP ( 'Fillet1', #3352 ) ;
#3321 = CARTESIAN_POINT ( 'NONE',  ( -40.45084971874737079, 41.98125000068279888, 29.38926261462367151 ) ) ;
#3322 = FACE_OUTER_BOUND ( 'NONE', #12290, .T. ) ;
#3323 = CARTESIAN_POINT ( 'NONE',  ( 0.000000000000000000, 217.0000000000000284, 0.000000000000000000 ) ) ;
#3324 = ORIENTED_EDGE ( 'NONE', *, *, #1297, .T. ) ;
#3325 = LINE ( 'NONE', #5831, #7558 ) ;
#3326 = LINE ( 'NONE', #902, #8216 ) ;
#3327 = DIRECTION ( 'NONE',  ( -0.000000000000000000, -1.000000000000000000, -0.000000000000000000 ) ) ;
#3328 = CARTESIAN_POINT ( 'NONE',  ( 0.000000000000000000, 22.50000000000000000, 101.0000000000000000 ) ) ;
#3329 = CARTESIAN_POINT ( 'NONE',  ( -3.407225380398804404, 31.38205016914259105, 101.0000000000000000 ) ) ;
#3330 = CARTESIAN_POINT ( 'NONE',  ( 38.60409515610501074, 25.00000000000000000, -31.77615201968907144 ) ) ;
#3331 = VECTOR ( 'NONE', #6236, 1000.000000000000000 ) ;
#3332 = CARTESIAN_POINT ( 'NONE',  ( -30.90169943749473447, 48.30000000000000426, 42.53254041760200721 ) ) ;
#3333 = CARTESIAN_POINT ( 'NONE',  ( -20.00000000000000711, 284.0710678118654755, -7.499999999999999112 ) ) ;
#3334 = PRESENTATION_LAYER_ASSIGNMENT (  '', '', ( #6543 ) ) ;
#3335 = CARTESIAN_POINT ( 'NONE',  ( -45.80914010100533318, 19.99999999999998934, 19.69865795820142296 ) ) ;
#3336 = CARTESIAN_POINT ( 'NONE',  ( 40.34137639590981905, 24.72187500034139873, 29.30972558990010768 ) ) ;
#3337 = CARTESIAN_POINT ( 'NONE',  ( 0.000000000000000000, 52.00000000000000711, 0.000000000000000000 ) ) ;
#3338 = CARTESIAN_POINT ( 'NONE',  ( -15.45084971874737256, 25.60000000000000142, -47.55282581475767500 ) ) ;
#3339 = CARTESIAN_POINT ( 'NONE',  ( 49.86468353125001585, 22.75937500034139660, 16.20201782572375038 ) ) ;
#3340 = CARTESIAN_POINT ( 'NONE',  ( 1.486087262401875941, 13.10364194761998213, 101.0000000000000000 ) ) ;
#3341 = ORIENTED_EDGE ( 'NONE', *, *, #9133, .T. ) ;
#3342 = VECTOR ( 'NONE', #474, 1000.000000000000000 ) ;
#3343 = VECTOR ( 'NONE', #15215, 1000.000000000000227 ) ;
#3344 = LINE ( 'NONE', #3435, #5713 ) ;
#3345 = ORIENTED_EDGE ( 'NONE', *, *, #15831, .T. ) ;
#3346 = STYLED_ITEM ( 'NONE', ( #2552 ), #7430 ) ;
#3347 = CARTESIAN_POINT ( 'NONE',  ( 0.000000000000000000, 261.9999999999999432, 0.000000000000000000 ) ) ;
#3348 = CARTESIAN_POINT ( 'NONE',  ( 15.40903463028481113, 33.25937500034140015, -47.42413220539094709 ) ) ;
#3349 = DIRECTION ( 'NONE',  ( 0.000000000000000000, 0.000000000000000000, -1.000000000000000000 ) ) ;
#3350 = CARTESIAN_POINT ( 'NONE',  ( 49.99999999999999289, 35.10000000000000853, -16.24598481164532160 ) ) ;
#3351 = DIRECTION ( 'NONE',  ( -0.000000000000000000, -1.000000000000000000, -0.000000000000000000 ) ) ;
#3352 = CLOSED_SHELL ( 'NONE', ( #340, #9425, #15061, #4596, #4600, #11997, #15540, #5614, #13028, #2865, #5348, #4130, #1831, #11349, #7416, #15151, #9005, #1139, #10596, #10379, #6482, #5246, #11840, #1524, #11929, #9065, #5107, #13308, #4482, #13095, #9438, #11226, #5373, #2857, #2046, #13588, #6077, #518, #7037, #12212, #1037, #7763, #1376, #7530, #142, #6647, #6327, #1109, #7467, #3681, #7130, #9163, #5608, #12112, #14525, #10180, #12714, #14320, #14720, #6203, #2698, #2301, #12507, #12901, #1662, #1859, #15961, #4443, #10602, #10069, #13449, #4386, #7968, #3277, #1033, #7787, #1115, #6416, #4197, #10285, #2557, #9876, #11225, #5615, #12804, #3291 ) ) ;
#3353 = CARTESIAN_POINT ( 'NONE',  ( 9.631387414534489405E-15, 30.42187500034139447, 52.43083105670540789 ) ) ;
#3354 = CARTESIAN_POINT ( 'NONE',  ( 15.40903463028482356, 26.45937500034139589, 47.42413220539093999 ) ) ;
#3355 = AXIS2_PLACEMENT_3D ( 'NONE', #10740, #1991, #4768 ) ;
#3356 = AXIS2_PLACEMENT_3D ( 'NONE', #8664, #9761, #845 ) ;
#3357 = DIRECTION ( 'NONE',  ( 0.8660254037844433705, 0.000000000000000000, 0.4999999999999916178 ) ) ;
#3358 = CARTESIAN_POINT ( 'NONE',  ( 40.34137639590981905, 30.72187500034139518, 29.30972558990010768 ) ) ;
#3359 = CARTESIAN_POINT ( 'NONE',  ( 0.000000000000000000, 257.0000000000001137, 0.000000000000000000 ) ) ;
#3360 = CARTESIAN_POINT ( 'NONE',  ( -15.40903463028481646, 43.45937500034139589, -47.42413220539093999 ) ) ;
#3361 = CARTESIAN_POINT ( 'NONE',  ( 49.86468353125000164, 34.92187500034140157, -6.106662507704105588E-15 ) ) ;
#3362 = EDGE_CURVE ( 'NONE', #566, #4055, #833, .T. ) ;
#3363 = EDGE_CURVE ( 'NONE', #7238, #10689, #3326, .T. ) ;
#3364 = CARTESIAN_POINT ( 'NONE',  ( -30.90169943749474868, 49.70000000000000284, -42.53254041760200721 ) ) ;
#3365 = ORIENTED_EDGE ( 'NONE', *, *, #8445, .T. ) ;
#3366 = CARTESIAN_POINT ( 'NONE',  ( 9.631387414534489405E-15, 42.35937500034140157, 52.43083105670540789 ) ) ;
#3367 = AXIS2_PLACEMENT_3D ( 'NONE', #15719, #9087, #6775 ) ;
#3368 = EDGE_LOOP ( 'NONE', ( #3979, #7984, #15935, #2640 ) ) ;
#3371 = ADVANCED_FACE ( 'NONE', ( #14786 ), #11066, .T. ) ;
#3370 = CARTESIAN_POINT ( 'NONE',  ( 49.99999999999999289, 24.88125000068279746, -16.24598481164532160 ) ) ;
#3369 = VECTOR ( 'NONE', #13704, 1000.000000000000000 ) ;
#3372 = EDGE_CURVE ( 'NONE', #1863, #7138, #8788, .T. ) ;
#3373 = EDGE_LOOP ( 'NONE', ( #1581, #13261, #7070, #7212 ) ) ;
#3374 = EDGE_CURVE ( 'NONE', #9264, #11588, #9646, .T. ) ;
#3375 = CARTESIAN_POINT ( 'NONE',  ( 1.293669679204937499E-13, 41.28125000068279604, -50.00000000000000000 ) ) ;
#3376 = CARTESIAN_POINT ( 'NONE',  ( 30.81806926056962936, 41.22187500034139873, -42.41743335407646498 ) ) ;
#3377 = CARTESIAN_POINT ( 'NONE',  ( 40.34137639590981905, 48.72187500034139873, 29.30972558990010768 ) ) ;
#3378 = CARTESIAN_POINT ( 'NONE',  ( 7.919222016226693306, 30.55125428154684286, 50.00000000000003553 ) ) ;
#3379 = CARTESIAN_POINT ( 'NONE',  ( -3.210462471511496205E-15, 21.42187500034139802, -52.43083105670540789 ) ) ;
#3380 = CARTESIAN_POINT ( 'NONE',  ( -3.219174618344376363E-15, 35.28125000068280315, -52.57311121191334990 ) ) ;
#3381 = CARTESIAN_POINT ( 'NONE',  ( 30.90169943749474157, 39.30000000000000426, -42.53254041760200721 ) ) ;
#3382 = AXIS2_PLACEMENT_3D ( 'NONE', #15114, #7559, #8719 ) ;
#3383 = CARTESIAN_POINT ( 'NONE',  ( -40.34137639590981905, 37.72187500034139873, -29.30972558990011478 ) ) ;
#3384 = CARTESIAN_POINT ( 'NONE',  ( -29.50911996093393341, 282.0000000000000000, -12.00911996094034961 ) ) ;
#3385 = ORIENTED_EDGE ( 'NONE', *, *, #15871, .F. ) ;
#3386 = CARTESIAN_POINT ( 'NONE',  ( 9.631387414534489405E-15, 42.42187500034140157, 52.43083105670540789 ) ) ;
#3387 = CARTESIAN_POINT ( 'NONE',  ( -5.823736356558307894E-14, 44.28125000068280315, 50.00000000000000000 ) ) ;
#3388 = ORIENTED_EDGE ( 'NONE', *, *, #1841, .T. ) ;
#3389 = ORIENTED_EDGE ( 'NONE', *, *, #7533, .T. ) ;
#3390 = VECTOR ( 'NONE', #13536, 999.9999999999998863 ) ;
#3391 = VERTEX_POINT ( 'NONE', #7081 ) ;
#3392 = EDGE_CURVE ( 'NONE', #16058, #13965, #8169, .T. ) ;
#3393 = CARTESIAN_POINT ( 'NONE',  ( -7.919222016226870942, 40.22999571913594963, 49.99999999999997158 ) ) ;
#3394 = FACE_OUTER_BOUND ( 'NONE', #8230, .T. ) ;
#3395 = CARTESIAN_POINT ( 'NONE',  ( 15.45084971874736723, 27.40000000000000213, -47.55282581475768211 ) ) ;
#3396 = PLANE ( 'NONE',  #12957 ) ;
#3397 = CARTESIAN_POINT ( 'NONE',  ( -49.86468353125000164, 37.85937500034139447, 0.000000000000000000 ) ) ;
#3398 = CARTESIAN_POINT ( 'NONE',  ( -15.40903463028480580, 48.25937500034140015, 47.42413220539094709 ) ) ;
#3399 = ADVANCED_FACE ( 'NONE', ( #10311 ), #8889, .F. ) ;
#3400 = CARTESIAN_POINT ( 'NONE',  ( -0.5000000000000000000, 245.0000000000000284, 49.99999999999999289 ) ) ;
#3401 = CARTESIAN_POINT ( 'NONE',  ( -1.671572875253809487, 242.8284271247462129, 49.99999999999999289 ) ) ;
#3402 = CARTESIAN_POINT ( 'NONE',  ( 0.000000000000000000, 22.50000000000000000, 101.0000000000000000 ) ) ;
#3403 = DIRECTION ( 'NONE',  ( -0.000000000000000000, -1.000000000000000000, -0.000000000000000000 ) ) ;
#3404 = CARTESIAN_POINT ( 'NONE',  ( -40.45084971874737789, 33.80000000000000426, -29.38926261462365730 ) ) ;
#3405 = CARTESIAN_POINT ( 'NONE',  ( -5.988468393965924008, 15.10823117958422301, 101.0000000000000000 ) ) ;
#3406 = VERTEX_POINT ( 'NONE', #4926 ) ;
#3407 =( BOUNDED_CURVE ( )  B_SPLINE_CURVE ( 2, ( #5885, #2455, #13762, #9949, #16341, #7458, #15004, #4638, #13677, #3642, #12525, #8696, #6213 ),
 .UNSPECIFIED., .F., .F. ) 
 B_SPLINE_CURVE_WITH_KNOTS ( ( 3, 2, 2, 2, 2, 2, 3 ),
 ( 0.2500000000000000000, 0.2533333333333333548, 0.2600000000000000089, 0.2666666666666666630, 0.2733333333333333171, 0.2800000000000000266, 0.2833333333333333814 ),
 .UNSPECIFIED. ) 
 CURVE ( )  GEOMETRIC_REPRESENTATION_ITEM ( )  RATIONAL_B_SPLINE_CURVE ( ( 0.9755282581475765991, 0.9755282581475765991, 1.000000000000000000, 0.9510565162951535312, 1.000000000000000000, 0.9510565162951535312, 1.000000000000000000, 0.9510565162951535312, 1.000000000000000000, 0.9510565162951535312, 1.000000000000000000, 0.9755282581475765991, 0.9755282581475768211 ) ) 
 REPRESENTATION_ITEM ( '' )  );
#3408 = CARTESIAN_POINT ( 'NONE',  ( 49.86468353124999453, 32.95937500034138168, -16.20201782572376459 ) ) ;
#3409 = ORIENTED_EDGE ( 'NONE', *, *, #2651, .T. ) ;
#3410 = ORIENTED_EDGE ( 'NONE', *, *, #11996, .T. ) ;
#3411 = ORIENTED_EDGE ( 'NONE', *, *, #8538, .T. ) ;
#3412 = CARTESIAN_POINT ( 'NONE',  ( -30.90169943749474868, 43.48125000068279178, -42.53254041760200721 ) ) ;
#3413 = CARTESIAN_POINT ( 'NONE',  ( 30.90169943749475223, 46.69999999999999574, 42.53254041760199300 ) ) ;
#3414 = CARTESIAN_POINT ( 'NONE',  ( 16.34981105473766760, 20.27881147257189909, 102.0000000000000142 ) ) ;
#3415 = ORIENTED_EDGE ( 'NONE', *, *, #15135, .F. ) ;
#3416 = DIRECTION ( 'NONE',  ( -0.000000000000000000, 1.000000000000000000, -0.000000000000000000 ) ) ;
#3417 = CARTESIAN_POINT ( 'NONE',  ( -3.111920190527341144E-15, 27.28125000068279604, -50.00000000000000000 ) ) ;
#3418 = AXIS2_PLACEMENT_3D ( 'NONE', #15258, #16350, #16194 ) ;
#3419 = CARTESIAN_POINT ( 'NONE',  ( -2.547328955960238000E-13, 20.49999999999999645, 49.99999999999999289 ) ) ;
#3420 = CARTESIAN_POINT ( 'NONE',  ( 2.500000000000000000, 247.0000000000000284, 47.99999999999999289 ) ) ;
#3421 = FACE_OUTER_BOUND ( 'NONE', #920, .T. ) ;
#3422 = CARTESIAN_POINT ( 'NONE',  ( 0.000000000000000000, 272.0000000000000000, 0.000000000000000000 ) ) ;
#3423 = ADVANCED_FACE ( 'NONE', ( #8804 ), #11392, .F. ) ;
#3424 = FACE_OUTER_BOUND ( 'NONE', #5431, .T. ) ;
#3425 = ADVANCED_FACE ( 'NONE', ( #2483 ), #9980, .F. ) ;
#3426 =( NAMED_UNIT ( * ) SI_UNIT ( $, .STERADIAN. ) SOLID_ANGLE_UNIT ( ) );
#3427 = CARTESIAN_POINT ( 'NONE',  ( 0.5000000000000000000, 245.0000000000000284, -49.99999999999999289 ) ) ;
#3428 = CARTESIAN_POINT ( 'NONE',  ( 9.631387414534489405E-15, 20.42187500034139447, 52.43083105670540789 ) ) ;
#3429 = CARTESIAN_POINT ( 'NONE',  ( 9.227956911499398113E-15, 102.0000000000000142, -1.913737646857611713E-14 ) ) ;
#3430 = CARTESIAN_POINT ( 'NONE',  ( 40.45084971874737079, 29.19999999999999929, -29.38926261462366440 ) ) ;
#3431 = CARTESIAN_POINT ( 'NONE',  ( -40.34137639590981195, 26.05937500034139731, 29.30972558990012189 ) ) ;
#3432 = CARTESIAN_POINT ( 'NONE',  ( -15.45084971874736368, 42.18125000068279462, 47.55282581475768211 ) ) ;
#3433 = CARTESIAN_POINT ( 'NONE',  ( -15.45084971874736368, 30.40000000000000213, 47.55282581475768211 ) ) ;
#3434 = EDGE_LOOP ( 'NONE', ( #6959, #1307, #15382, #3013 ) ) ;
#3435 = CARTESIAN_POINT ( 'NONE',  ( 5.179451399591075145, 14.52044592729181538, 101.0000000000000000 ) ) ;
#3436 = ORIENTED_EDGE ( 'NONE', *, *, #11535, .T. ) ;
#3437 = CARTESIAN_POINT ( 'NONE',  ( 30.81806926056964002, 34.55937500034139731, 42.41743335407647209 ) ) ;
#3438 = DIRECTION ( 'NONE',  ( -0.000000000000000000, -1.000000000000000000, -0.000000000000000000 ) ) ;
#3439 = DIRECTION ( 'NONE',  ( -0.000000000000000000, 0.000000000000000000, 1.000000000000000000 ) ) ;
#3440 = LINE ( 'NONE', #2172, #7521 ) ;
#3441 = CARTESIAN_POINT ( 'NONE',  ( 0.000000000000000000, 20.00000000000000355, -10.00000000000000000 ) ) ;
#3442 = PRESENTATION_LAYER_ASSIGNMENT (  '', '', ( #5827 ) ) ;
#3443 = CARTESIAN_POINT ( 'NONE',  ( -3.210462471511496205E-15, 29.42187500034139092, -52.43083105670540789 ) ) ;
#3444 = CARTESIAN_POINT ( 'NONE',  ( -30.81806926056963292, 29.55937500034139376, -42.41743335407646498 ) ) ;
#3445 = LINE ( 'NONE', #6028, #16395 ) ;
#3446 = CARTESIAN_POINT ( 'NONE',  ( 49.86468353125001585, 30.82187500034139660, 16.20201782572375038 ) ) ;
#3447 = CARTESIAN_POINT ( 'NONE',  ( 40.45084971874737789, 32.80000000000000426, 29.38926261462365375 ) ) ;
#3448 = CARTESIAN_POINT ( 'NONE',  ( 15.40903463028481113, 45.25937500034140015, -47.42413220539094709 ) ) ;
#3449 = CARTESIAN_POINT ( 'NONE',  ( 30.81806926056964002, 36.62187500034139731, 42.41743335407647209 ) ) ;
#3450 = CARTESIAN_POINT ( 'NONE',  ( -15.45084971874737256, 49.60000000000000853, -47.55282581475767500 ) ) ;
#3451 = ORIENTED_EDGE ( 'NONE', *, *, #5460, .F. ) ;
#3452 = AXIS2_PLACEMENT_3D ( 'NONE', #8398, #5997, #5915 ) ;
#3453 = CARTESIAN_POINT ( 'NONE',  ( -15.40903463028480580, 42.25937500034139305, 47.42413220539094709 ) ) ;
#3454 = ORIENTED_EDGE ( 'NONE', *, *, #11284, .T. ) ;
#3455 = CARTESIAN_POINT ( 'NONE',  ( -49.99999999999999289, 25.68125000068279462, -16.24598481164531449 ) ) ;
#3456 = VERTEX_POINT ( 'NONE', #2653 ) ;
#3457 = CARTESIAN_POINT ( 'NONE',  ( 50.00000000000000711, 40.68125000068280173, 16.24598481164530739 ) ) ;
#3458 = CARTESIAN_POINT ( 'NONE',  ( -15.40903463028480580, 40.32187500034140015, 47.42413220539094709 ) ) ;
#3459 = CARTESIAN_POINT ( 'NONE',  ( -30.81806926056963292, 21.55937500034140086, -42.41743335407647209 ) ) ;
#3460 = CARTESIAN_POINT ( 'NONE',  ( 40.45084971874737789, 40.80000000000000426, 29.38926261462365375 ) ) ;
#3461 = CARTESIAN_POINT ( 'NONE',  ( -40.34137639590981905, 25.72187500034139518, -29.30972558990011478 ) ) ;
#3462 = CONTEXT_DEPENDENT_SHAPE_REPRESENTATION ( #471, #11975 ) ;
#3463 = CARTESIAN_POINT ( 'NONE',  ( -40.45084971874737789, 31.58125000068280031, -29.38926261462365730 ) ) ;
#3464 = EDGE_CURVE ( 'NONE', #9110, #1819, #13528, .T. ) ;
#3465 = EDGE_CURVE ( 'NONE', #14577, #6674, #9030, .T. ) ;
#3466 = CARTESIAN_POINT ( 'NONE',  ( 49.86468353125001585, 42.82187500034139305, 16.20201782572375038 ) ) ;
#3467 = CARTESIAN_POINT ( 'NONE',  ( 6.123233995736766085E-15, 193.4213562373095385, 50.00000000000000000 ) ) ;
#3468 = EDGE_LOOP ( 'NONE', ( #3472, #15630, #4022, #16418 ) ) ;
#3469 = CARTESIAN_POINT ( 'NONE',  ( 9.631387414534489405E-15, 36.42187500034139447, 52.43083105670540789 ) ) ;
#3470 = CARTESIAN_POINT ( 'NONE',  ( -7.919222016226816763, 43.33250428222963535, -49.99999999999999289 ) ) ;
#3471 = ADVANCED_FACE ( 'NONE', ( #6329 ), #15195, .T. ) ;
#3472 = ORIENTED_EDGE ( 'NONE', *, *, #7941, .F. ) ;
#3473 = VERTEX_POINT ( 'NONE', #3742 ) ;
#3474 = ORIENTED_EDGE ( 'NONE', *, *, #5567, .T. ) ;
#3475 = CARTESIAN_POINT ( 'NONE',  ( -40.45084971874737079, 39.98125000068279888, 29.38926261462367151 ) ) ;
#3476 = CARTESIAN_POINT ( 'NONE',  ( 17.50000000000000000, 22.50000000000000355, 80.00000000000000000 ) ) ;
#3477 = EDGE_CURVE ( 'NONE', #8881, #9739, #3909, .T. ) ;
#3478 = DIRECTION ( 'NONE',  ( 0.000000000000000000, 0.000000000000000000, -1.000000000000000000 ) ) ;
#3479 = CARTESIAN_POINT ( 'NONE',  ( 9.657523855033129090E-15, 20.50000000000000355, 52.57311121191334990 ) ) ;
#3480 = CARTESIAN_POINT ( 'NONE',  ( -49.86468353125000164, 35.85937500034140157, 0.000000000000000000 ) ) ;
#3481 = CARTESIAN_POINT ( 'NONE',  ( 15.40903463028482356, 48.45937500034140299, 47.42413220539093999 ) ) ;
#3482 = DIRECTION ( 'NONE',  ( -0.000000000000000000, -0.000000000000000000, -1.000000000000000000 ) ) ;
#3483 = DIRECTION ( 'NONE',  ( 0.8660254037844433705, 0.000000000000000000, 0.4999999999999918399 ) ) ;
#3484 =( NAMED_UNIT ( * ) PLANE_ANGLE_UNIT ( ) SI_UNIT ( $, .RADIAN. ) );
#3485 = CARTESIAN_POINT ( 'NONE',  ( 9.227956911499398113E-15, 102.0000000000000142, -1.913737646857611713E-14 ) ) ;
#3486 = CARTESIAN_POINT ( 'NONE',  ( -30.90169943749473447, 46.30000000000000426, 42.53254041760200721 ) ) ;
#3487 = DIRECTION ( 'NONE',  ( 1.000000000000000000, 0.000000000000000000, -0.000000000000000000 ) ) ;
#3488 = EDGE_LOOP ( 'NONE', ( #13018, #12960, #9890, #4639 ) ) ;
#3489 = EDGE_CURVE ( 'NONE', #15672, #5969, #2323, .T. ) ;
#3490 = CARTESIAN_POINT ( 'NONE',  ( 40.34137639590981905, 26.65937500034139518, 29.30972558990010768 ) ) ;
#3491 = ORIENTED_EDGE ( 'NONE', *, *, #2957, .T. ) ;
#3492 = VERTEX_POINT ( 'NONE', #7650 ) ;
#3493 = ORIENTED_EDGE ( 'NONE', *, *, #9782, .T. ) ;
#3494 = CARTESIAN_POINT ( 'NONE',  ( 30.90169943749475578, 46.48125000068280599, 42.53254041760200010 ) ) ;
#3495 = FACE_OUTER_BOUND ( 'NONE', #6655, .T. ) ;
#3496 = CARTESIAN_POINT ( 'NONE',  ( 0.000000000000000000, 267.0000000000000000, 0.000000000000000000 ) ) ;
#3497 = EDGE_CURVE ( 'NONE', #14319, #11849, #13789, .T. ) ;
#3498 = ORIENTED_EDGE ( 'NONE', *, *, #10033, .F. ) ;
#3499 = DIRECTION ( 'NONE',  ( -0.000000000000000000, -0.000000000000000000, -1.000000000000000000 ) ) ;
#3500 = FILL_AREA_STYLE_COLOUR ( '', #9281 ) ;
#3501 = CARTESIAN_POINT ( 'NONE',  ( -17.36041212498391673, 20.22110460638136331, 94.85899783816353192 ) ) ;
#3502 = LINE ( 'NONE', #5262, #8940 ) ;
#3503 = FACE_OUTER_BOUND ( 'NONE', #5085, .T. ) ;
#3504 = CARTESIAN_POINT ( 'NONE',  ( -20.00000000000000355, 307.0000000000000568, 2.500000000000001332 ) ) ;
#3505 = DIRECTION ( 'NONE',  ( 0.000000000000000000, 0.000000000000000000, -1.000000000000000000 ) ) ;
#3506 = DIRECTION ( 'NONE',  ( 0.000000000000000000, -0.000000000000000000, 1.000000000000000000 ) ) ;
#3507 = PLANE ( 'NONE',  #8590 ) ;
#3508 = CARTESIAN_POINT ( 'NONE',  ( -30.90169943749473802, 44.08125000068279320, 42.53254041760200721 ) ) ;
#3509 =( BOUNDED_CURVE ( )  B_SPLINE_CURVE ( 2, ( #8487, #12230, #12402, #12307, #12150, #13310, #5924, #994, #13631, #11162, #9748, #14793, #13553 ),
 .UNSPECIFIED., .F., .T. ) 
 B_SPLINE_CURVE_WITH_KNOTS ( ( 3, 2, 2, 2, 2, 2, 3 ),
 ( 0.2500000000000000000, 0.2533333333333333548, 0.2600000000000000089, 0.2666666666666666630, 0.2733333333333333171, 0.2800000000000000266, 0.2833333333333333814 ),
 .UNSPECIFIED. ) 
 CURVE ( )  GEOMETRIC_REPRESENTATION_ITEM ( )  RATIONAL_B_SPLINE_CURVE ( ( 0.9755282581475765991, 0.9755282581475765991, 1.000000000000000000, 0.9510565162951535312, 1.000000000000000000, 0.9510565162951535312, 1.000000000000000000, 0.9510565162951535312, 1.000000000000000000, 0.9510565162951535312, 1.000000000000000000, 0.9755282581475765991, 0.9755282581475768211 ) ) 
 REPRESENTATION_ITEM ( '' )  );
#3510 = DIRECTION ( 'NONE',  ( 1.000000000000000000, 0.000000000000000000, 0.000000000000000000 ) ) ;
#3511 = CARTESIAN_POINT ( 'NONE',  ( -30.90169943749473802, 26.29999999999999716, 42.53254041760200721 ) ) ;
#3512 = CARTESIAN_POINT ( 'NONE',  ( -49.86468353124999453, 21.75937500034140015, -16.20201782572375393 ) ) ;
#3513 = DIRECTION ( 'NONE',  ( 0.000000000000000000, 0.000000000000000000, 1.000000000000000000 ) ) ;
#3514 = CARTESIAN_POINT ( 'NONE',  ( -30.90169943749474513, 29.69999999999999929, -42.53254041760200721 ) ) ;
#3515 = EDGE_LOOP ( 'NONE', ( #13115, #3081, #8654, #8363 ) ) ;
#3516 = CARTESIAN_POINT ( 'NONE',  ( 7.919222016226791006, 44.55125428154683931, 50.00000000000000711 ) ) ;
#3517 = EDGE_LOOP ( 'NONE', ( #14869, #5824, #12490, #11784 ) ) ;
#3518 = DIRECTION ( 'NONE',  ( 0.8660254037844362651, 0.5000000000000041078, 0.000000000000000000 ) ) ;
#3519 = CARTESIAN_POINT ( 'NONE',  ( 40.34137639590981905, 32.65937500034139873, 29.30972558990010768 ) ) ;
#3520 = CARTESIAN_POINT ( 'NONE',  ( -29.32979127811529096, 20.09142360399907190, 43.04328433925359576 ) ) ;
#3521 = CARTESIAN_POINT ( 'NONE',  ( -49.99999999999999289, 49.68125000068279462, -16.24598481164531449 ) ) ;
#3522 = DIRECTION ( 'NONE',  ( -0.000000000000000000, -1.000000000000000000, -0.000000000000000000 ) ) ;
#3523 = DIRECTION ( 'NONE',  ( 0.000000000000000000, 0.000000000000000000, -1.000000000000000000 ) ) ;
#3524 = CARTESIAN_POINT ( 'NONE',  ( -49.86468353125000164, 23.92187500034139447, 0.000000000000000000 ) ) ;
#3525 = CARTESIAN_POINT ( 'NONE',  ( 30.81806926056962936, 31.15937500034139163, -42.41743335407646498 ) ) ;
#3526 = CARTESIAN_POINT ( 'NONE',  ( 50.00000000000000711, 26.68125000068279462, 16.24598481164530739 ) ) ;
#3527 = CARTESIAN_POINT ( 'NONE',  ( -3.210462471511496205E-15, 37.42187500034140157, -52.43083105670540789 ) ) ;
#3528 = CARTESIAN_POINT ( 'NONE',  ( 4.890515327186548689, 101.5721353500714059, -8.487905985326074543 ) ) ;
#3529 = CARTESIAN_POINT ( 'NONE',  ( -15.40903463028481646, 45.45937500034139589, -47.42413220539093999 ) ) ;
#3530 = CARTESIAN_POINT ( 'NONE',  ( -15.40903463028480580, 36.32187500034140015, 47.42413220539094709 ) ) ;
#3531 = AXIS2_PLACEMENT_3D ( 'NONE', #12865, #12783, #1304 ) ;
#3532 = CARTESIAN_POINT ( 'NONE',  ( 49.99999999999999289, 47.10000000000000853, -16.24598481164532160 ) ) ;
#3533 = ORIENTED_EDGE ( 'NONE', *, *, #16361, .T. ) ;
#3534 = CARTESIAN_POINT ( 'NONE',  ( 49.86468353125000164, 42.85937500034140157, -6.106662507704105588E-15 ) ) ;
#3535 = EDGE_CURVE ( 'NONE', #14691, #14151, #5850, .T. ) ;
#3536 = ORIENTED_EDGE ( 'NONE', *, *, #8529, .F. ) ;
#3537 = CARTESIAN_POINT ( 'NONE',  ( -3.219174618344376363E-15, 27.28125000068279249, -52.57311121191334990 ) ) ;
#3538 = ORIENTED_EDGE ( 'NONE', *, *, #5207, .T. ) ;
#3539 = VECTOR ( 'NONE', #5938, 1000.000000000000000 ) ;
#3540 = DIRECTION ( 'NONE',  ( 1.000000000000000000, 0.000000000000000000, 0.000000000000000000 ) ) ;
#3541 = CARTESIAN_POINT ( 'NONE',  ( -3.210462471511496205E-15, 47.42187500034138736, -52.43083105670540789 ) ) ;
#3542 = SPHERICAL_SURFACE ( 'NONE', #8622, 5.000000000000000000 ) ;
#3543 = CARTESIAN_POINT ( 'NONE',  ( -30.81806926056962226, 24.22187500034139163, 42.41743335407647919 ) ) ;
#3544 = EDGE_CURVE ( 'NONE', #15116, #11630, #1147, .T. ) ;
#3545 = CARTESIAN_POINT ( 'NONE',  ( 9.657523855033129090E-15, 36.28125000068278894, 52.57311121191334990 ) ) ;
#3546 = CARTESIAN_POINT ( 'NONE',  ( 49.86468353124999453, 43.02187500034138878, -16.20201782572376459 ) ) ;
#3547 = CARTESIAN_POINT ( 'NONE',  ( -28.70358715772690061, 282.1599167565163384, -9.907174315453927349 ) ) ;
#3548 = EDGE_LOOP ( 'NONE', ( #9663, #10724, #4831, #16342 ) ) ;
#3549 = VECTOR ( 'NONE', #10900, 1000.000000000000000 ) ;
#3550 = CARTESIAN_POINT ( 'NONE',  ( -49.86468353124999453, 36.02187500034139589, 16.20201782572377525 ) ) ;
#3551 = CARTESIAN_POINT ( 'NONE',  ( -30.90169943749473447, 32.08125000068280031, 42.53254041760200721 ) ) ;
#3552 = ORIENTED_EDGE ( 'NONE', *, *, #8040, .F. ) ;
#3553 = ORIENTED_EDGE ( 'NONE', *, *, #8956, .T. ) ;
#3554 = ORIENTED_EDGE ( 'NONE', *, *, #14421, .F. ) ;
#3555 = EDGE_CURVE ( 'NONE', #11555, #891, #8750, .T. ) ;
#3556 = DIRECTION ( 'NONE',  ( 0.5000000000000041078, -0.8660254037844363761, -0.000000000000000000 ) ) ;
#3557 = CARTESIAN_POINT ( 'NONE',  ( -16.79120288457607657, 27.43006142852237517, 101.0000000000000000 ) ) ;
#3558 = FACE_OUTER_BOUND ( 'NONE', #1478, .T. ) ;
#3559 = DIRECTION ( 'NONE',  ( 1.000000000000000000, -0.000000000000000000, 1.734723475976807094E-17 ) ) ;
#3560 = CARTESIAN_POINT ( 'NONE',  ( -30.81806926056963292, 39.55937500034139731, -42.41743335407647209 ) ) ;
#3561 = CARTESIAN_POINT ( 'NONE',  ( 15.40903463028481113, 45.25937500034140015, -47.42413220539094709 ) ) ;
#3562 = CARTESIAN_POINT ( 'NONE',  ( 40.45084971874737079, 25.19999999999999929, -29.38926261462366440 ) ) ;
#3563 = VECTOR ( 'NONE', #12126, 999.9999999999998863 ) ;
#3564 = CARTESIAN_POINT ( 'NONE',  ( 0.000000000000000000, 25.00000000000000355, 0.000000000000000000 ) ) ;
#3565 = CARTESIAN_POINT ( 'NONE',  ( 13.33959974903368995, 33.83821319854147447, 101.0000000000000000 ) ) ;
#3566 = CARTESIAN_POINT ( 'NONE',  ( -1.240322475938754499E-13, 36.50000000000000711, 50.00000000000000000 ) ) ;
#3567 = PLANE ( 'NONE',  #6457 ) ;
#3568 = ORIENTED_EDGE ( 'NONE', *, *, #14634, .T. ) ;
#3569 = ADVANCED_FACE ( 'NONE', ( #11232 ), #16377, .F. ) ;
#3570 = CARTESIAN_POINT ( 'NONE',  ( -49.86468353124999453, 25.95937500034139944, 16.20201782572377525 ) ) ;
#3571 = CARTESIAN_POINT ( 'NONE',  ( 8.446640517145639571E-15, 48.28125000068279604, 50.00000000000000000 ) ) ;
#3572 = ORIENTED_EDGE ( 'NONE', *, *, #2125, .F. ) ;
#3573 = EDGE_LOOP ( 'NONE', ( #7136, #645, #15857, #5332 ) ) ;
#3574 = AXIS2_PLACEMENT_3D ( 'NONE', #2074, #8009, #1608 ) ;
#3575 = CARTESIAN_POINT ( 'NONE',  ( -15.45084971874736368, 40.18125000068280173, 47.55282581475768211 ) ) ;
#3576 = CYLINDRICAL_SURFACE ( 'NONE', #2570, 2.000000000000001776 ) ;
#3577 = FILL_AREA_STYLE_COLOUR ( '', #1974 ) ;
#3578 = ORIENTED_EDGE ( 'NONE', *, *, #2254, .F. ) ;
#3579 = CARTESIAN_POINT ( 'NONE',  ( -40.45084971874737789, 27.58125000068280031, -29.38926261462365730 ) ) ;
#3580 = FACE_OUTER_BOUND ( 'NONE', #5253, .T. ) ;
#3581 = DIRECTION ( 'NONE',  ( 0.000000000000000000, 0.000000000000000000, 1.000000000000000000 ) ) ;
#3582 = CARTESIAN_POINT ( 'NONE',  ( 0.000000000000000000, 272.0000000000000000, 0.000000000000000000 ) ) ;
#3583 = CARTESIAN_POINT ( 'NONE',  ( 0.000000000000000000, 20.00000000000000355, 0.000000000000000000 ) ) ;
#3584 = FACE_OUTER_BOUND ( 'NONE', #11947, .T. ) ;
#3585 = EDGE_CURVE ( 'NONE', #5800, #7317, #15393, .T. ) ;
#3586 = CARTESIAN_POINT ( 'NONE',  ( 30.90169943749475223, 36.48125000068279888, 42.53254041760199300 ) ) ;
#3587 = CARTESIAN_POINT ( 'NONE',  ( 0.000000000000000000, 20.00000000000000355, 0.000000000000000000 ) ) ;
#3588 = CARTESIAN_POINT ( 'NONE',  ( 30.90169943749474157, 45.08125000068279320, -42.53254041760200721 ) ) ;
#3589 = DIRECTION ( 'NONE',  ( 0.9777979793268661846, -0.2095497831645198317, 0.000000000000000000 ) ) ;
#3590 = CIRCLE ( 'NONE', #8089, 17.50000000000000000 ) ;
#3591 = CARTESIAN_POINT ( 'NONE',  ( 50.00000000000000711, 28.89999999999999858, 16.24598481164530739 ) ) ;
#3592 = CARTESIAN_POINT ( 'NONE',  ( 49.86468353125000164, 20.85937500034139802, -6.106662507704105588E-15 ) ) ;
#3593 = CARTESIAN_POINT ( 'NONE',  ( 7.513064459987437071E-14, 42.50000000000000000, 50.00000000000000000 ) ) ;
#3594 = CARTESIAN_POINT ( 'NONE',  ( 30.81806926056964002, 46.55937500034139020, 42.41743335407647209 ) ) ;
#3595 = ORIENTED_EDGE ( 'NONE', *, *, #2982, .T. ) ;
#3596 = FACE_OUTER_BOUND ( 'NONE', #7045, .T. ) ;
#3597 = ORIENTED_EDGE ( 'NONE', *, *, #1100, .F. ) ;
#3598 = DIRECTION ( 'NONE',  ( 0.000000000000000000, -1.000000000000000000, 0.000000000000000000 ) ) ;
#3599 = CARTESIAN_POINT ( 'NONE',  ( 30.81806926056964002, 36.55937500034139731, 42.41743335407647209 ) ) ;
#3600 = CIRCLE ( 'NONE', #1192, 79.49773270518484480 ) ;
#3601 = CARTESIAN_POINT ( 'NONE',  ( 30.90169943749475223, 40.48125000068279888, 42.53254041760199300 ) ) ;
#3602 = DIRECTION ( 'NONE',  ( -0.000000000000000000, -1.000000000000000000, -0.000000000000000000 ) ) ;
#3603 = EDGE_CURVE ( 'NONE', #4080, #9526, #1047, .T. ) ;
#3604 = CARTESIAN_POINT ( 'NONE',  ( 0.000000000000000000, 52.26146722824297797, 62.01141590572476758 ) ) ;
#3605 =( BOUNDED_SURFACE ( )  B_SPLINE_SURFACE ( 1, 2, ( 
 ( #8205, #15760, #11776, #4141, #14351, #543, #13273, #4388, #3133, #9124, #6651, #300, #6567, #11865, #7959, #6810, #10457, #10629, #11625, #2893, #10378, #13196, #222, #4229, #11700, #11944, #377, #5327, #5397, #15513, #14184, #9216, #2968, #465, #9452, #4308, #2800, #14269, #9373, #8116, #13032, #14508, #9298, #8036, #1800, #7876, #1634, #6729, #5479, #12953, #1557, #14424, #13109, #10551, #15607, #6892, #3044, #5635, #1714, #10700, #5568, #6968, #12103, #7294, #1872, #14836, #791, #9699, #11122, #3546, #15930, #3466, #11028, #12020, #620, #12190, #8523, #712, #5881, #5716, #2117, #10786, #10943, #9615, #4552, #7206, #13513, #14663, #869, #15852, #3293, #951, #12350, #1951, #16183, #4474, #4634, #8599, #5965, #8361, #16096, #9540, #10866, #4812, #8449, #12267, #13592, #13350, #9865, #2197, #14585, #6052, #3211, #14916, #8282, #13432, #7043, #16008, #5796, #2042, #7131, #14749, #3383, #4731, #9789, #1288, #4889, #13759, #6295, #8776, #5065, #2286, #15339, #15089, #7378, #12444, #7531, #10197, #7455, #12602, #1035, #13918, #6132, #1196, #4977, #16338, #2537, #8860, #10037, #12691, #13674, #3717, #12770, #7700, #2372, #6460, #11203, #16431, #3956, #6381, #11280, #11443, #16255, #6209, #11518, #3796, #7617, #15250, #8693, #5225, #3876, #9946, #8949, #15001, #116, #3637, #13838, #12522, #11364, #1368, #1113, #2452, #10117, #15168, #10282, #36, #5141, #14005, #2624, #1618, #4122, #361, #14085, #10687, #10441, #15741, #6877, #5625, #1452, #9108, #2784, #9031, #14335, #15497, #9280, #12937, #13094, #2701, #5384, #12848, #15670, #7777, #6711, #14167, #14406, #2875, #6544, #7858, #1543, #203, #6632, #5464, #2951, #11928, #6796, #11606, #282, #11845, #10613, #11684, #530, #11762, #10530, #4293, #5309, #9195, #14254, #7942, #10359, #15419, #1699, #15588, #4038, #13015, #9355, #450, #8100, #4213, #13178, #8018, #5551, #3029, #1784, #4370, #857, #3278, #12175, #13577, #6035, #1936, #5950, #13497, #7028, #13256, #604, #11107, #7117, #7192, #9437, #5865, #12083, #13409, #690, #4538, #2182, #774, #7278, #11011, #5783, #12254, #3119, #9525, #12335, #10850, #15915, #9601, #4711, #16076, #8512, #14571, #8346, #8191, #14648, #4617, #2023, #10928, #9773, #15992, #2104, #9681, #14819 ),
 ( #8433, #14731, #3195, #3364, #3450, #936, #6953, #14487, #1856, #12007, #5697, #10767, #15830, #4459, #8268, #13333, #8840, #16414, #4876, #9933, #11267, #7513, #12583, #11426, #3856, #14986, #13822, #9852, #8924, #3532, #5047, #12673, #10100, #15074, #16324, #11348, #6362, #6439, #4796, #8584, #1270, #12430, #11189, #2268, #5124, #13987, #4961, #8679, #19, #15152, #1022, #13900, #7365, #16167, #10177, #14904, #2359, #13658, #8761, #10021, #15227, #3703, #12751, #16242, #2435, #2605, #7441, #7681, #6118, #1099, #1180, #3616, #1348, #6277, #13745, #12508, #3777, #2515, #7597, #6193, #3939, #15319, #9012, #12829, #14068, #1431, #7758, #2684, #11500, #97, #5201, #10259, #8281, #12102, #708, #11264, #1096, #15071, #15850, #9614, #9451, #5795, #10942, #3290, #13347, #6189, #10864, #3381, #7129, #13742, #618, #7508, #4385, #8448, #4633, #3132, #16007, #9697, #14662, #14748, #7042, #9538, #13431, #16321, #7438, #13272, #12580, #3700, #15929, #1949, #2040, #4956, #4551, #12187, #5715, #2355, #12504, #4473, #14584, #8360, #790, #5880, #10017, #8757, #3209, #13819, #14504, #2431, #8204, #1177, #10699, #15757, #1870, #6966, #12019, #10783, #12995, #11345, #15148, #2761, #2512, #1267, #8833, #11665, #10422, #11497, #15223, #1521, #11577, #7591, #4019, #13897, #6272, #7837, #16411, #8918, #5044, #15316, #6436, #5366, #5197, #2852, #6359, #3936, #9169, #13984, #6610, #10097, #7678, #2681, #10173, #261, #9008, #12911, #12670, #14065, #10253, #1345, #2601, #12748, #3774, #11423, #7919, #7755, #9088, #16, #12825, #94, #1428, #5120, #3853, #15476, #6518, #4098, #183, #5287, #14227, #10338, #15399, #14145, #1810, #15447, #2816, #1569, #5411, #10469, #4319, #10639, #8134, #9137, #2904, #2728, #15527, #4241, #13044, #6662, #15691, #4157, #13120, #390, #6824, #10391, #553, #14113, #1727, #14361, #12878, #9308, #2978, #7972, #8048, #311, #7890, #6743, #9384, #475, #6581, #5646, #13206, #9229, #11712, #11790, #14434, #14282, #5494, #4065, #11877, #5578, #14196, #12965, #1646, #10563, #15616, #3057, #6901, #11955, #10712, #7806, #3988, #1484, #9060, #11638, #232, #5339, #15940, #10955, #5975, #6064, #4398, #8215, #12279, #12030, #10802, #1885, #4743, #3479, #4562, #8293, #11041, #4648, #632 ) ),
 .UNSPECIFIED., .F., .F., .T. ) 
 B_SPLINE_SURFACE_WITH_KNOTS ( ( 2, 2 ),
 ( 3, 2, 2, 2, 2, 2, 2, 2, 2, 2, 2, 2, 2, 2, 2, 2, 2, 2, 2, 2, 2, 2, 2, 2, 2, 2, 2, 2, 2, 2, 2, 2, 2, 2, 2, 2, 2, 2, 2, 2, 2, 2, 2, 2, 2, 2, 2, 2, 2, 2, 2, 2, 2, 2, 2, 2, 2, 2, 2, 2, 2, 2, 2, 2, 2, 2, 2, 2, 2, 2, 2, 2, 2, 2, 2, 2, 2, 2, 2, 2, 2, 2, 2, 2, 2, 2, 2, 2, 2, 2, 2, 2, 2, 2, 2, 2, 2, 2, 2, 2, 2, 2, 2, 2, 2, 2, 2, 2, 2, 2, 2, 2, 2, 2, 2, 2, 2, 2, 2, 2, 2, 2, 2, 2, 2, 2, 2, 2, 2, 2, 2, 2, 2, 2, 2, 2, 2, 2, 2, 2, 2, 2, 2, 2, 2, 2, 2, 2, 2, 2, 3 ),
 ( 0.000000000000000000, 1.000000000000000000 ),
 ( 0.000000000000000000, 0.006666666666666667095, 0.01333333333333333419, 0.02000000000000000042, 0.02666666666666666838, 0.03333333333333333287, 0.04000000000000000083, 0.04666666666666666879, 0.05333333333333333676, 0.05999999999999999778, 0.06666666666666666574, 0.07333333333333333370, 0.08000000000000000167, 0.08666666666666666963, 0.09333333333333333759, 0.1000000000000000056, 0.1066666666666666735, 0.1133333333333333276, 0.1199999999999999956, 0.1266666666666666774, 0.1333333333333333315, 0.1400000000000000133, 0.1466666666666666674, 0.1533333333333333215, 0.1600000000000000033, 0.1666666666666666574, 0.1733333333333333393, 0.1799999999999999933, 0.1866666666666666752, 0.1933333333333333293, 0.2000000000000000111, 0.2066666666666666652, 0.2133333333333333470, 0.2200000000000000011, 0.2266666666666666552, 0.2333333333333333370, 0.2399999999999999911, 0.2466666666666666730, 0.2533333333333333548, 0.2600000000000000089, 0.2666666666666666630, 0.2733333333333333171, 0.2800000000000000266, 0.2866666666666666807, 0.2933333333333333348, 0.2999999999999999889, 0.3066666666666666430, 0.3133333333333333526, 0.3200000000000000067, 0.3266666666666666607, 0.3333333333333333148, 0.3400000000000000244, 0.3466666666666666785, 0.3533333333333333326, 0.3599999999999999867, 0.3666666666666666408, 0.3733333333333333504, 0.3800000000000000044, 0.3866666666666666585, 0.3933333333333333126, 0.4000000000000000222, 0.4066666666666666763, 0.4133333333333333304, 0.4199999999999999845, 0.4266666666666666941, 0.4333333333333333481, 0.4400000000000000022, 0.4466666666666666563, 0.4533333333333333104, 0.4600000000000000200, 0.4666666666666666741, 0.4733333333333333282, 0.4799999999999999822, 0.4866666666666666918, 0.4933333333333333459, 0.5000000000000000000, 0.5066666666666667096, 0.5133333333333333082, 0.5200000000000000178, 0.5266666666666666163, 0.5333333333333333259, 0.5400000000000000355, 0.5466666666666666341, 0.5533333333333333437, 0.5600000000000000533, 0.5666666666666666519, 0.5733333333333333615, 0.5799999999999999600, 0.5866666666666666696, 0.5933333333333333792, 0.5999999999999999778, 0.6066666666666666874, 0.6133333333333332860, 0.6199999999999999956, 0.6266666666666667052, 0.6333333333333333037, 0.6400000000000000133, 0.6466666666666666119, 0.6533333333333333215, 0.6600000000000000311, 0.6666666666666666297, 0.6733333333333333393, 0.6800000000000000488, 0.6866666666666666474, 0.6933333333333333570, 0.6999999999999999556, 0.7066666666666666652, 0.7133333333333333748, 0.7199999999999999734, 0.7266666666666666829, 0.7333333333333332815, 0.7399999999999999911, 0.7466666666666667007, 0.7533333333333332993, 0.7600000000000000089, 0.7666666666666667185, 0.7733333333333333171, 0.7800000000000000266, 0.7866666666666666252, 0.7933333333333333348, 0.8000000000000000444, 0.8066666666666666430, 0.8133333333333333526, 0.8199999999999999512, 0.8266666666666666607, 0.8333333333333333703, 0.8399999999999999689, 0.8466666666666666785, 0.8533333333333333881, 0.8599999999999999867, 0.8666666666666666963, 0.8733333333333332948, 0.8800000000000000044, 0.8866666666666667140, 0.8933333333333333126, 0.9000000000000000222, 0.9066666666666666208, 0.9133333333333333304, 0.9200000000000000400, 0.9266666666666666385, 0.9333333333333333481, 0.9399999999999999467, 0.9466666666666666563, 0.9533333333333333659, 0.9599999999999999645, 0.9666666666666666741, 0.9733333333333333837, 0.9799999999999999822, 0.9866666666666666918, 0.9933333333333332904, 1.000000000000000000 ),
 .UNSPECIFIED. ) 
 GEOMETRIC_REPRESENTATION_ITEM ( )  RATIONAL_B_SPLINE_SURFACE ( (
 ( 1.000000000000000000, 0.9510565162951535312, 1.000000000000000000, 0.9510565162951535312, 1.000000000000000000, 0.9510565162951535312, 1.000000000000000000, 0.9510565162951535312, 1.000000000000000000, 0.9510565162951535312, 1.000000000000000000, 0.9510565162951535312, 1.000000000000000000, 0.9510565162951535312, 1.000000000000000000, 0.9510565162951535312, 1.000000000000000000, 0.9510565162951535312, 1.000000000000000000, 0.9510565162951535312, 1.000000000000000000, 0.9510565162951535312, 1.000000000000000000, 0.9510565162951535312, 1.000000000000000000, 0.9510565162951535312, 1.000000000000000000, 0.9510565162951535312, 1.000000000000000000, 0.9510565162951535312, 1.000000000000000000, 0.9510565162951535312, 1.000000000000000000, 0.9510565162951535312, 1.000000000000000000, 0.9510565162951535312, 1.000000000000000000, 0.9510565162951535312, 1.000000000000000000, 0.9510565162951535312, 1.000000000000000000, 0.9510565162951535312, 1.000000000000000000, 0.9510565162951535312, 1.000000000000000000, 0.9510565162951535312, 1.000000000000000000, 0.9510565162951535312, 1.000000000000000000, 0.9510565162951535312, 1.000000000000000000, 0.9510565162951535312, 1.000000000000000000, 0.9510565162951535312, 1.000000000000000000, 0.9510565162951535312, 1.000000000000000000, 0.9510565162951535312, 1.000000000000000000, 0.9510565162951535312, 1.000000000000000000, 0.9510565162951535312, 1.000000000000000000, 0.9510565162951535312, 1.000000000000000000, 0.9510565162951535312, 1.000000000000000000, 0.9510565162951535312, 1.000000000000000000, 0.9510565162951535312, 1.000000000000000000, 0.9510565162951535312, 1.000000000000000000, 0.9510565162951535312, 1.000000000000000000, 0.9510565162951535312, 1.000000000000000000, 0.9510565162951535312, 1.000000000000000000, 0.9510565162951535312, 1.000000000000000000, 0.9510565162951535312, 1.000000000000000000, 0.9510565162951535312, 1.000000000000000000, 0.9510565162951535312, 1.000000000000000000, 0.9510565162951535312, 1.000000000000000000, 0.9510565162951535312, 1.000000000000000000, 0.9510565162951535312, 1.000000000000000000, 0.9510565162951535312, 1.000000000000000000, 0.9510565162951535312, 1.000000000000000000, 0.9510565162951535312, 1.000000000000000000, 0.9510565162951535312, 1.000000000000000000, 0.9510565162951535312, 1.000000000000000000, 0.9510565162951535312, 1.000000000000000000, 0.9510565162951535312, 1.000000000000000000, 0.9510565162951535312, 1.000000000000000000, 0.9510565162951535312, 1.000000000000000000, 0.9510565162951535312, 1.000000000000000000, 0.9510565162951535312, 1.000000000000000000, 0.9510565162951535312, 1.000000000000000000, 0.9510565162951535312, 1.000000000000000000, 0.9510565162951535312, 1.000000000000000000, 0.9510565162951535312, 1.000000000000000000, 0.9510565162951535312, 1.000000000000000000, 0.9510565162951535312, 1.000000000000000000, 0.9510565162951535312, 1.000000000000000000, 0.9510565162951535312, 1.000000000000000000, 0.9510565162951535312, 1.000000000000000000, 0.9510565162951535312, 1.000000000000000000, 0.9510565162951535312, 1.000000000000000000, 0.9510565162951535312, 1.000000000000000000, 0.9510565162951535312, 1.000000000000000000, 0.9510565162951535312, 1.000000000000000000, 0.9510565162951535312, 1.000000000000000000, 0.9510565162951535312, 1.000000000000000000, 0.9510565162951535312, 1.000000000000000000, 0.9510565162951535312, 1.000000000000000000, 0.9510565162951535312, 1.000000000000000000, 0.9510565162951535312, 1.000000000000000000, 0.9510565162951535312, 1.000000000000000000, 0.9510565162951535312, 1.000000000000000000, 0.9510565162951535312, 1.000000000000000000, 0.9510565162951535312, 1.000000000000000000, 0.9510565162951535312, 1.000000000000000000, 0.9510565162951535312, 1.000000000000000000, 0.9510565162951535312, 1.000000000000000000, 0.9510565162951535312, 1.000000000000000000, 0.9510565162951535312, 1.000000000000000000, 0.9510565162951535312, 1.000000000000000000, 0.9510565162951535312, 1.000000000000000000, 0.9510565162951535312, 1.000000000000000000, 0.9510565162951535312, 1.000000000000000000, 0.9510565162951535312, 1.000000000000000000, 0.9510565162951535312, 1.000000000000000000, 0.9510565162951535312, 1.000000000000000000, 0.9510565162951535312, 1.000000000000000000, 0.9510565162951535312, 1.000000000000000000, 0.9510565162951535312, 1.000000000000000000, 0.9510565162951535312, 1.000000000000000000, 0.9510565162951535312, 1.000000000000000000, 0.9510565162951535312, 1.000000000000000000, 0.9510565162951535312, 1.000000000000000000, 0.9510565162951535312, 1.000000000000000000, 0.9510565162951535312, 1.000000000000000000, 0.9510565162951535312, 1.000000000000000000, 0.9510565162951535312, 1.000000000000000000, 0.9510565162951535312, 1.000000000000000000, 0.9510565162951535312, 1.000000000000000000, 0.9510565162951535312, 1.000000000000000000, 0.9510565162951535312, 1.000000000000000000, 0.9510565162951535312, 1.000000000000000000, 0.9510565162951535312, 1.000000000000000000, 0.9510565162951535312, 1.000000000000000000, 0.9510565162951535312, 1.000000000000000000, 0.9510565162951535312, 1.000000000000000000, 0.9510565162951535312, 1.000000000000000000, 0.9510565162951535312, 1.000000000000000000, 0.9510565162951535312, 1.000000000000000000, 0.9510565162951535312, 1.000000000000000000, 0.9510565162951535312, 1.000000000000000000, 0.9510565162951535312, 1.000000000000000000, 0.9510565162951535312, 1.000000000000000000, 0.9510565162951535312, 1.000000000000000000, 0.9510565162951535312, 1.000000000000000000, 0.9510565162951535312, 1.000000000000000000, 0.9510565162951535312, 1.000000000000000000, 0.9510565162951535312, 1.000000000000000000, 0.9510565162951535312, 1.000000000000000000, 0.9510565162951535312, 1.000000000000000000, 0.9510565162951535312, 1.000000000000000000, 0.9510565162951535312, 1.000000000000000000, 0.9510565162951535312, 1.000000000000000000, 0.9510565162951535312, 1.000000000000000000, 0.9510565162951535312, 1.000000000000000000, 0.9510565162951535312, 1.000000000000000000, 0.9510565162951535312, 1.000000000000000000, 0.9510565162951535312, 1.000000000000000000, 0.9510565162951535312, 1.000000000000000000, 0.9510565162951535312, 1.000000000000000000, 0.9510565162951535312, 1.000000000000000000, 0.9510565162951535312, 1.000000000000000000, 0.9510565162951535312, 1.000000000000000000, 0.9510565162951535312, 1.000000000000000000, 0.9510565162951535312, 1.000000000000000000, 0.9510565162951535312, 1.000000000000000000, 0.9510565162951535312, 1.000000000000000000, 0.9510565162951535312, 1.000000000000000000, 0.9510565162951535312, 1.000000000000000000, 0.9510565162951535312, 1.000000000000000000, 0.9510565162951535312, 1.000000000000000000, 0.9510565162951535312, 1.000000000000000000, 0.9510565162951535312, 1.000000000000000000),
 ( 1.000000000000000000, 0.9510565162951535312, 1.000000000000000000, 0.9510565162951535312, 1.000000000000000000, 0.9510565162951535312, 1.000000000000000000, 0.9510565162951535312, 1.000000000000000000, 0.9510565162951535312, 1.000000000000000000, 0.9510565162951535312, 1.000000000000000000, 0.9510565162951535312, 1.000000000000000000, 0.9510565162951535312, 1.000000000000000000, 0.9510565162951535312, 1.000000000000000000, 0.9510565162951535312, 1.000000000000000000, 0.9510565162951535312, 1.000000000000000000, 0.9510565162951535312, 1.000000000000000000, 0.9510565162951535312, 1.000000000000000000, 0.9510565162951535312, 1.000000000000000000, 0.9510565162951535312, 1.000000000000000000, 0.9510565162951535312, 1.000000000000000000, 0.9510565162951535312, 1.000000000000000000, 0.9510565162951535312, 1.000000000000000000, 0.9510565162951535312, 1.000000000000000000, 0.9510565162951535312, 1.000000000000000000, 0.9510565162951535312, 1.000000000000000000, 0.9510565162951535312, 1.000000000000000000, 0.9510565162951535312, 1.000000000000000000, 0.9510565162951535312, 1.000000000000000000, 0.9510565162951535312, 1.000000000000000000, 0.9510565162951535312, 1.000000000000000000, 0.9510565162951535312, 1.000000000000000000, 0.9510565162951535312, 1.000000000000000000, 0.9510565162951535312, 1.000000000000000000, 0.9510565162951535312, 1.000000000000000000, 0.9510565162951535312, 1.000000000000000000, 0.9510565162951535312, 1.000000000000000000, 0.9510565162951535312, 1.000000000000000000, 0.9510565162951535312, 1.000000000000000000, 0.9510565162951535312, 1.000000000000000000, 0.9510565162951535312, 1.000000000000000000, 0.9510565162951535312, 1.000000000000000000, 0.9510565162951535312, 1.000000000000000000, 0.9510565162951535312, 1.000000000000000000, 0.9510565162951535312, 1.000000000000000000, 0.9510565162951535312, 1.000000000000000000, 0.9510565162951535312, 1.000000000000000000, 0.9510565162951535312, 1.000000000000000000, 0.9510565162951535312, 1.000000000000000000, 0.9510565162951535312, 1.000000000000000000, 0.9510565162951535312, 1.000000000000000000, 0.9510565162951535312, 1.000000000000000000, 0.9510565162951535312, 1.000000000000000000, 0.9510565162951535312, 1.000000000000000000, 0.9510565162951535312, 1.000000000000000000, 0.9510565162951535312, 1.000000000000000000, 0.9510565162951535312, 1.000000000000000000, 0.9510565162951535312, 1.000000000000000000, 0.9510565162951535312, 1.000000000000000000, 0.9510565162951535312, 1.000000000000000000, 0.9510565162951535312, 1.000000000000000000, 0.9510565162951535312, 1.000000000000000000, 0.9510565162951535312, 1.000000000000000000, 0.9510565162951535312, 1.000000000000000000, 0.9510565162951535312, 1.000000000000000000, 0.9510565162951535312, 1.000000000000000000, 0.9510565162951535312, 1.000000000000000000, 0.9510565162951535312, 1.000000000000000000, 0.9510565162951535312, 1.000000000000000000, 0.9510565162951535312, 1.000000000000000000, 0.9510565162951535312, 1.000000000000000000, 0.9510565162951535312, 1.000000000000000000, 0.9510565162951535312, 1.000000000000000000, 0.9510565162951535312, 1.000000000000000000, 0.9510565162951535312, 1.000000000000000000, 0.9510565162951535312, 1.000000000000000000, 0.9510565162951535312, 1.000000000000000000, 0.9510565162951535312, 1.000000000000000000, 0.9510565162951535312, 1.000000000000000000, 0.9510565162951535312, 1.000000000000000000, 0.9510565162951535312, 1.000000000000000000, 0.9510565162951535312, 1.000000000000000000, 0.9510565162951535312, 1.000000000000000000, 0.9510565162951535312, 1.000000000000000000, 0.9510565162951535312, 1.000000000000000000, 0.9510565162951535312, 1.000000000000000000, 0.9510565162951535312, 1.000000000000000000, 0.9510565162951535312, 1.000000000000000000, 0.9510565162951535312, 1.000000000000000000, 0.9510565162951535312, 1.000000000000000000, 0.9510565162951535312, 1.000000000000000000, 0.9510565162951535312, 1.000000000000000000, 0.9510565162951535312, 1.000000000000000000, 0.9510565162951535312, 1.000000000000000000, 0.9510565162951535312, 1.000000000000000000, 0.9510565162951535312, 1.000000000000000000, 0.9510565162951535312, 1.000000000000000000, 0.9510565162951535312, 1.000000000000000000, 0.9510565162951535312, 1.000000000000000000, 0.9510565162951535312, 1.000000000000000000, 0.9510565162951535312, 1.000000000000000000, 0.9510565162951535312, 1.000000000000000000, 0.9510565162951535312, 1.000000000000000000, 0.9510565162951535312, 1.000000000000000000, 0.9510565162951535312, 1.000000000000000000, 0.9510565162951535312, 1.000000000000000000, 0.9510565162951535312, 1.000000000000000000, 0.9510565162951535312, 1.000000000000000000, 0.9510565162951535312, 1.000000000000000000, 0.9510565162951535312, 1.000000000000000000, 0.9510565162951535312, 1.000000000000000000, 0.9510565162951535312, 1.000000000000000000, 0.9510565162951535312, 1.000000000000000000, 0.9510565162951535312, 1.000000000000000000, 0.9510565162951535312, 1.000000000000000000, 0.9510565162951535312, 1.000000000000000000, 0.9510565162951535312, 1.000000000000000000, 0.9510565162951535312, 1.000000000000000000, 0.9510565162951535312, 1.000000000000000000, 0.9510565162951535312, 1.000000000000000000, 0.9510565162951535312, 1.000000000000000000, 0.9510565162951535312, 1.000000000000000000, 0.9510565162951535312, 1.000000000000000000, 0.9510565162951535312, 1.000000000000000000, 0.9510565162951535312, 1.000000000000000000, 0.9510565162951535312, 1.000000000000000000, 0.9510565162951535312, 1.000000000000000000, 0.9510565162951535312, 1.000000000000000000, 0.9510565162951535312, 1.000000000000000000, 0.9510565162951535312, 1.000000000000000000, 0.9510565162951535312, 1.000000000000000000, 0.9510565162951535312, 1.000000000000000000, 0.9510565162951535312, 1.000000000000000000, 0.9510565162951535312, 1.000000000000000000, 0.9510565162951535312, 1.000000000000000000, 0.9510565162951535312, 1.000000000000000000, 0.9510565162951535312, 1.000000000000000000, 0.9510565162951535312, 1.000000000000000000, 0.9510565162951535312, 1.000000000000000000, 0.9510565162951535312, 1.000000000000000000, 0.9510565162951535312, 1.000000000000000000, 0.9510565162951535312, 1.000000000000000000, 0.9510565162951535312, 1.000000000000000000, 0.9510565162951535312, 1.000000000000000000, 0.9510565162951535312, 1.000000000000000000, 0.9510565162951535312, 1.000000000000000000, 0.9510565162951535312, 1.000000000000000000, 0.9510565162951535312, 1.000000000000000000, 0.9510565162951535312, 1.000000000000000000, 0.9510565162951535312, 1.000000000000000000, 0.9510565162951535312, 1.000000000000000000, 0.9510565162951535312, 1.000000000000000000, 0.9510565162951535312, 1.000000000000000000, 0.9510565162951535312, 1.000000000000000000, 0.9510565162951535312, 1.000000000000000000) ) ) 
 REPRESENTATION_ITEM ( '' )  SURFACE ( )  );
#3606 = CARTESIAN_POINT ( 'NONE',  ( 7.513064459987437071E-14, 42.28125000068280315, 50.00000000000000000 ) ) ;
#3607 = EDGE_CURVE ( 'NONE', #15466, #1879, #8976, .T. ) ;
#3608 = CARTESIAN_POINT ( 'NONE',  ( -15.40903463028480580, 20.32187500034139660, 47.42413220539094709 ) ) ;
#3609 = CARTESIAN_POINT ( 'NONE',  ( 15.40903463028482356, 32.45937500034138878, 47.42413220539093999 ) ) ;
#3610 = CARTESIAN_POINT ( 'NONE',  ( 17.50000000000000000, 22.50000000000000355, 80.00000000000000000 ) ) ;
#3611 = CARTESIAN_POINT ( 'NONE',  ( 30.81806926056964002, 32.62187500034140442, 42.41743335407646498 ) ) ;
#3612 = PLANE ( 'NONE',  #11861 ) ;
#3613 = CARTESIAN_POINT ( 'NONE',  ( -49.86468353124999453, 41.75937500034139305, -16.20201782572375393 ) ) ;
#3614 = CARTESIAN_POINT ( 'NONE',  ( -40.34137639590981195, 36.12187500034139731, 29.30972558990012189 ) ) ;
#3615 = AXIS2_PLACEMENT_3D ( 'NONE', #5188, #1417, #5035 ) ;
#3616 = CARTESIAN_POINT ( 'NONE',  ( 50.00000000000000711, 42.89999999999999858, 16.24598481164530739 ) ) ;
#3617 =( GEOMETRIC_REPRESENTATION_CONTEXT ( 3 ) GLOBAL_UNCERTAINTY_ASSIGNED_CONTEXT ( ( #7760 ) ) GLOBAL_UNIT_ASSIGNED_CONTEXT ( ( #3062, #11717, #11960 ) ) REPRESENTATION_CONTEXT ( 'NONE', 'WORKASPACE' ) );
#3618 = ORIENTED_EDGE ( 'NONE', *, *, #4491, .T. ) ;
#3619 = CARTESIAN_POINT ( 'NONE',  ( 49.86468353125001585, 40.75937500034138594, 16.20201782572375038 ) ) ;
#3620 = VECTOR ( 'NONE', #1929, 1000.000000000000114 ) ;
#3621 = VERTEX_POINT ( 'NONE', #7725 ) ;
#3622 = CARTESIAN_POINT ( 'NONE',  ( 50.00000000000000711, 26.68125000068279462, 16.24598481164530739 ) ) ;
#3623 = DIRECTION ( 'NONE',  ( 0.000000000000000000, 1.000000000000000000, 0.000000000000000000 ) ) ;
#3624 = VECTOR ( 'NONE', #15715, 1000.000000000000000 ) ;
#3625 = CIRCLE ( 'NONE', #12915, 45.00000000000000000 ) ;
#3626 = CIRCLE ( 'NONE', #5750, 45.00000000000000000 ) ;
#3627 = CIRCLE ( 'NONE', #16086, 5.000000000000000888 ) ;
#3628 = CARTESIAN_POINT ( 'NONE',  ( -40.45084971874737789, 35.79999999999999716, -29.38926261462365730 ) ) ;
#3629 = CARTESIAN_POINT ( 'NONE',  ( 49.86468353125001585, 42.82187500034139305, 16.20201782572375038 ) ) ;
#3630 = AXIS2_PLACEMENT_3D ( 'NONE', #2799, #6564, #14267 ) ;
#3631 = FACE_OUTER_BOUND ( 'NONE', #1957, .T. ) ;
#3632 = EDGE_CURVE ( 'NONE', #436, #11764, #1979, .T. ) ;
#3633 = CARTESIAN_POINT ( 'NONE',  ( 15.40903463028481113, 21.32187500034139660, -47.42413220539094709 ) ) ;
#3634 = EDGE_CURVE ( 'NONE', #11764, #8121, #4104, .T. ) ;
#3635 = CARTESIAN_POINT ( 'NONE',  ( -50.00000000000000000, 25.78125000068279959, 0.000000000000000000 ) ) ;
#3636 = MANIFOLD_SOLID_BREP ( 'Cut-Extrude1', #13180 ) ;
#3637 = CARTESIAN_POINT ( 'NONE',  ( 9.631387414534489405E-15, 32.42187500034139447, 52.43083105670540789 ) ) ;
#3638 = CARTESIAN_POINT ( 'NONE',  ( -25.15991675646742465, 285.7035871579729474, -2.819833512935953301 ) ) ;
#3639 = CIRCLE ( 'NONE', #15298, 17.50000000000000000 ) ;
#3640 = VECTOR ( 'NONE', #12630, 1000.000000000000000 ) ;
#3641 = CARTESIAN_POINT ( 'NONE',  ( 49.86468353125000164, 34.92187500034140157, -6.106662507704105588E-15 ) ) ;
#3642 = CARTESIAN_POINT ( 'NONE',  ( -30.90169943749474513, 41.48125000068279178, -42.53254041760200721 ) ) ;
#3643 = ORIENTED_EDGE ( 'NONE', *, *, #2037, .T. ) ;
#3644 = VERTEX_POINT ( 'NONE', #61 ) ;
#3645 = EDGE_LOOP ( 'NONE', ( #7472, #10327, #10768, #13301 ) ) ;
#3646 = PLANE ( 'NONE',  #1519 ) ;
#3647 = CARTESIAN_POINT ( 'NONE',  ( 17.11764542475610185, 21.20361710786393417, 101.3333374614808662 ) ) ;
#3648 = CARTESIAN_POINT ( 'NONE',  ( -40.45084971874737079, 23.98125000068279888, 29.38926261462367151 ) ) ;
#3649 = VECTOR ( 'NONE', #15870, 1000.000000000000000 ) ;
#3650 = CARTESIAN_POINT ( 'NONE',  ( -30.81806926056962226, 32.15937500034139873, 42.41743335407647919 ) ) ;
#3651 = CARTESIAN_POINT ( 'NONE',  ( 9.631387414534489405E-15, 40.35937500034139447, 52.43083105670540789 ) ) ;
#3652 = AXIS2_PLACEMENT_3D ( 'NONE', #3266, #5388, #15424 ) ;
#3653 = CYLINDRICAL_SURFACE ( 'NONE', #5764, 42.00000000000000711 ) ;
#3654 = PLANE ( 'NONE',  #8592 ) ;
#3655 = CARTESIAN_POINT ( 'NONE',  ( -7.919222016226816763, 35.33250428222964246, -49.99999999999999289 ) ) ;
#3656 = SURFACE_STYLE_FILL_AREA ( #12620 ) ;
#3657 = EDGE_LOOP ( 'NONE', ( #5872, #13522, #6637, #8547 ) ) ;
#3658 = CARTESIAN_POINT ( 'NONE',  ( 49.86468353125001585, 26.75937500034139660, 16.20201782572375038 ) ) ;
#3659 = LINE ( 'NONE', #8715, #5745 ) ;
#3660 = ORIENTED_EDGE ( 'NONE', *, *, #7533, .F. ) ;
#3661 = ORIENTED_EDGE ( 'NONE', *, *, #9501, .F. ) ;
#3662 = CARTESIAN_POINT ( 'NONE',  ( 50.00000000000000000, 34.78125000068280315, -6.123233995736766085E-15 ) ) ;
#3663 = FACE_OUTER_BOUND ( 'NONE', #12089, .T. ) ;
#3664 = DIRECTION ( 'NONE',  ( -0.000000000000000000, -1.000000000000000000, -0.000000000000000000 ) ) ;
#3665 = ORIENTED_EDGE ( 'NONE', *, *, #3967, .F. ) ;
#3666 = DIRECTION ( 'NONE',  ( 0.3213938048432681271, -0.5817472440052512406, 0.7471788047720988590 ) ) ;
#3667 = DIRECTION ( 'NONE',  ( -0.000000000000000000, 0.000000000000000000, 1.000000000000000000 ) ) ;
#3668 = CARTESIAN_POINT ( 'NONE',  ( -7.919222016226934890, 20.44874571845315714, 49.99999999999996447 ) ) ;
#3669 = CARTESIAN_POINT ( 'NONE',  ( 0.000000000000000000, 22.50000000000000000, 102.0000000000000142 ) ) ;
#3670 = FACE_OUTER_BOUND ( 'NONE', #12240, .T. ) ;
#3671 = FACE_OUTER_BOUND ( 'NONE', #3573, .T. ) ;
#3672 = EDGE_CURVE ( 'NONE', #6301, #5249, #16457, .T. ) ;
#3673 = LINE ( 'NONE', #8729, #4421 ) ;
#3674 = AXIS2_PLACEMENT_3D ( 'NONE', #6394, #6226, #3897 ) ;
#3675 = DIRECTION ( 'NONE',  ( -0.000000000000000000, 1.000000000000000000, -0.000000000000000000 ) ) ;
#3676 = DIRECTION ( 'NONE',  ( 0.3420201433256698231, -0.6644630243886754384, -0.6644630243886734400 ) ) ;
#3677 = CARTESIAN_POINT ( 'NONE',  ( 15.45084971874736723, 45.18125000068280173, -47.55282581475768211 ) ) ;
#3678 = CARTESIAN_POINT ( 'NONE',  ( 15.45084971874736723, 31.39999999999999858, -47.55282581475768211 ) ) ;
#3679 = CARTESIAN_POINT ( 'NONE',  ( -49.99999999999999289, 25.89999999999999858, -16.24598481164531449 ) ) ;
#3680 = DIRECTION ( 'NONE',  ( 0.000000000000000000, 1.000000000000000000, 0.000000000000000000 ) ) ;
#3681 = ADVANCED_FACE ( 'NONE', ( #6486 ), #144, .F. ) ;
#3682 = EDGE_CURVE ( 'NONE', #14909, #383, #7971, .T. ) ;
#3683 = CARTESIAN_POINT ( 'NONE',  ( -30.81806926056963292, 43.55937500034139731, -42.41743335407647209 ) ) ;
#3684 = ORIENTED_EDGE ( 'NONE', *, *, #7766, .F. ) ;
#3685 = VECTOR ( 'NONE', #3559, 1000.000000000000000 ) ;
#3686 = EDGE_CURVE ( 'NONE', #3456, #5700, #1645, .T. ) ;
#3687 = EDGE_LOOP ( 'NONE', ( #8908, #8659, #937, #13226, #13943 ) ) ;
#3688 = CARTESIAN_POINT ( 'NONE',  ( -17.45639740057859868, 21.16801284050013976, 102.0000000000000142 ) ) ;
#3689 = CARTESIAN_POINT ( 'NONE',  ( 40.34137639590981195, 35.05937500034139731, -29.30972558990011834 ) ) ;
#3690 = DIRECTION ( 'NONE',  ( 0.000000000000000000, 0.000000000000000000, -1.000000000000000000 ) ) ;
#3691 = CARTESIAN_POINT ( 'NONE',  ( 0.000000000000000000, 22.50000000000000000, 102.0000000000000142 ) ) ;
#3692 = CARTESIAN_POINT ( 'NONE',  ( 46.91068958262674471, 25.00000000000000711, -16.90862634959390931 ) ) ;
#3693 = EDGE_CURVE ( 'NONE', #12352, #305, #15615, .T. ) ;
#3694 = CARTESIAN_POINT ( 'NONE',  ( 0.000000000000000000, 50.00000000000000000, 50.00000000000000000 ) ) ;
#3695 = CARTESIAN_POINT ( 'NONE',  ( -15.40903463028481646, 25.52187500034139589, -47.42413220539093999 ) ) ;
#3696 = CARTESIAN_POINT ( 'NONE',  ( 40.34137639590981905, 22.65937500034139518, 29.30972558990010768 ) ) ;
#3697 = CARTESIAN_POINT ( 'NONE',  ( 0.000000000000000000, 50.00000000000000000, 0.000000000000000000 ) ) ;
#3698 = CARTESIAN_POINT ( 'NONE',  ( 15.40903463028481113, 33.32187500034139305, -47.42413220539094709 ) ) ;
#3699 = CARTESIAN_POINT ( 'NONE',  ( -3.111920190527341144E-15, 29.28125000068279604, -50.00000000000000000 ) ) ;
#3700 = CARTESIAN_POINT ( 'NONE',  ( 30.90169943749474157, 37.30000000000000426, -42.53254041760200721 ) ) ;
#3701 = CARTESIAN_POINT ( 'NONE',  ( -40.34137639590981905, 41.65937500034139873, -29.30972558990011478 ) ) ;
#3702 = CARTESIAN_POINT ( 'NONE',  ( -40.34137639590981195, 30.12187500034139731, 29.30972558990012189 ) ) ;
#3703 = CARTESIAN_POINT ( 'NONE',  ( -49.99999999999999289, 43.90000000000000568, -16.24598481164531449 ) ) ;
#3704 = VERTEX_POINT ( 'NONE', #12029 ) ;
#3705 = CARTESIAN_POINT ( 'NONE',  ( 49.86468353125001585, 36.75937500034139305, 16.20201782572375038 ) ) ;
#3706 = ORIENTED_EDGE ( 'NONE', *, *, #12556, .T. ) ;
#3708 =( BOUNDED_CURVE ( )  B_SPLINE_CURVE ( 2, ( #3375, #2281, #6126, #5790, #13504, #16249, #5957, #3457, #12436, #11196, #14994, #2033, #1029 ),
 .UNSPECIFIED., .F., .F. ) 
 B_SPLINE_CURVE_WITH_KNOTS ( ( 3, 2, 2, 2, 2, 2, 3 ),
 ( 0.2833333333333333814, 0.2866666666666666807, 0.2933333333333333348, 0.2999999999999999889, 0.3066666666666666430, 0.3133333333333333526, 0.3166666666666667074 ),
 .UNSPECIFIED. ) 
 CURVE ( )  GEOMETRIC_REPRESENTATION_ITEM ( )  RATIONAL_B_SPLINE_CURVE ( ( 0.9755282581475768211, 0.9755282581475770431, 1.000000000000000000, 0.9510565162951535312, 1.000000000000000000, 0.9510565162951535312, 1.000000000000000000, 0.9510565162951535312, 1.000000000000000000, 0.9510565162951535312, 1.000000000000000000, 0.9755282581475765991, 0.9755282581475768211 ) ) 
 REPRESENTATION_ITEM ( '' )  );
#3707 = CARTESIAN_POINT ( 'NONE',  ( 30.90169943749474157, 25.08125000068279675, -42.53254041760200721 ) ) ;
#3709 = VECTOR ( 'NONE', #6145, 1000.000000000000000 ) ;
#3710 = DIRECTION ( 'NONE',  ( -0.9993309688977880523, -0.03657341386592528887, -0.000000000000000000 ) ) ;
#3711 = CARTESIAN_POINT ( 'NONE',  ( -40.34137639590981905, 25.72187500034139518, -29.30972558990011478 ) ) ;
#3712 = CARTESIAN_POINT ( 'NONE',  ( -49.86468353124999453, 44.02187500034139589, 16.20201782572377525 ) ) ;
#3713 = DIRECTION ( 'NONE',  ( 0.000000000000000000, 0.000000000000000000, -1.000000000000000000 ) ) ;
#3714 = CARTESIAN_POINT ( 'NONE',  ( -40.45084971874737079, 48.20000000000000284, 29.38926261462367151 ) ) ;
#3715 = CARTESIAN_POINT ( 'NONE',  ( 40.45084971874737789, 28.58125000068280031, 29.38926261462365375 ) ) ;
#3716 = AXIS2_PLACEMENT_3D ( 'NONE', #2572, #6405, #7726 ) ;
#3717 = CARTESIAN_POINT ( 'NONE',  ( 49.86468353125001585, 34.82187500034140015, 16.20201782572375038 ) ) ;
#3718 = DIRECTION ( 'NONE',  ( -0.000000000000000000, -1.000000000000000000, -0.000000000000000000 ) ) ;
#3719 = CARTESIAN_POINT ( 'NONE',  ( -49.86468353125000164, 37.92187500034140157, 0.000000000000000000 ) ) ;
#3720 = CARTESIAN_POINT ( 'NONE',  ( -40.45084971874737789, 31.58125000068280031, -29.38926261462365730 ) ) ;
#3721 = ORIENTED_EDGE ( 'NONE', *, *, #11682, .F. ) ;
#3722 = ORIENTED_EDGE ( 'NONE', *, *, #14933, .F. ) ;
#3723 = ADVANCED_FACE ( 'NONE', ( #8047 ), #7699, .T. ) ;
#3724 = DIRECTION ( 'NONE',  ( 0.000000000000000000, 0.000000000000000000, 1.000000000000000000 ) ) ;
#3725 = DIRECTION ( 'NONE',  ( 0.000000000000000000, 0.000000000000000000, -1.000000000000000000 ) ) ;
#3726 = DIRECTION ( 'NONE',  ( 0.8090169943749425663, 0.5877852522924799095, 0.000000000000000000 ) ) ;
#3727 = CARTESIAN_POINT ( 'NONE',  ( 5.000000000000000000, 102.2474899284555931, 10.24748992845553808 ) ) ;
#3728 = CARTESIAN_POINT ( 'NONE',  ( 40.34137639590981905, 32.65937500034139873, 29.30972558990010768 ) ) ;
#3729 = CARTESIAN_POINT ( 'NONE',  ( -15.40903463028480580, 46.32187500034140015, 47.42413220539094709 ) ) ;
#3730 = CARTESIAN_POINT ( 'NONE',  ( -49.99999999999999289, 39.90000000000000568, -16.24598481164531449 ) ) ;
#3731 = DIRECTION ( 'NONE',  ( 0.000000000000000000, 1.000000000000000000, 0.000000000000000000 ) ) ;
#3732 = CARTESIAN_POINT ( 'NONE',  ( -2.500000000000000000, 242.0000000000000284, -40.00000000000000000 ) ) ;
#3733 = ORIENTED_EDGE ( 'NONE', *, *, #5119, .T. ) ;
#3734 = CARTESIAN_POINT ( 'NONE',  ( -49.86468353124999453, 23.75937500034140015, -16.20201782572375393 ) ) ;
#3735 = ORIENTED_EDGE ( 'NONE', *, *, #4217, .T. ) ;
#3736 = CARTESIAN_POINT ( 'NONE',  ( 2.978552182361884590E-14, 47.28125000068279604, -50.00000000000000000 ) ) ;
#3737 = ORIENTED_EDGE ( 'NONE', *, *, #3374, .T. ) ;
#3738 = ORIENTED_EDGE ( 'NONE', *, *, #9953, .T. ) ;
#3739 = CARTESIAN_POINT ( 'NONE',  ( -7.977241335952133916, 17.31698729810774751, 102.0000000000000142 ) ) ;
#3740 = DIRECTION ( 'NONE',  ( -1.000000000000000000, 0.000000000000000000, 0.000000000000000000 ) ) ;
#3741 = CARTESIAN_POINT ( 'NONE',  ( 30.90169943749475223, 38.48125000068279888, 42.53254041760199300 ) ) ;
#3742 = CARTESIAN_POINT ( 'NONE',  ( -2.547328955960238000E-13, 32.28125000068278894, 49.99999999999999289 ) ) ;
#3743 = CARTESIAN_POINT ( 'NONE',  ( -30.81806926056963292, 47.55937500034139731, -42.41743335407647209 ) ) ;
#3744 = DIRECTION ( 'NONE',  ( 0.000000000000000000, 0.000000000000000000, 1.000000000000000000 ) ) ;
#3745 = CARTESIAN_POINT ( 'NONE',  ( 7.499999999999987566, 40.00000000000000711, -2.602085213965205908E-15 ) ) ;
#3746 = PLANE ( 'NONE',  #15092 ) ;
#3747 = CARTESIAN_POINT ( 'NONE',  ( 0.5000000000000001110, 38.99242250247064590, 102.0000000000000142 ) ) ;
#3748 = SHAPE_REPRESENTATION_RELATIONSHIP ( 'NONE' , 'NONE' ,  #9477, #3231 ) ;
#3749 = CARTESIAN_POINT ( 'NONE',  ( 25.00000000000000000, 287.0000000000000568, -2.499999999999997780 ) ) ;
#3750 = CARTESIAN_POINT ( 'NONE',  ( 50.00000000000000711, 46.68125000068278752, 16.24598481164530739 ) ) ;
#3751 = CARTESIAN_POINT ( 'NONE',  ( 21.27467419401223125, 99.27155792573854853, -5.000000000000000000 ) ) ;
#3752 = EDGE_CURVE ( 'NONE', #4896, #12984, #14596, .T. ) ;
#3753 = CARTESIAN_POINT ( 'NONE',  ( 15.45084971874736723, 47.18125000068280173, -47.55282581475768211 ) ) ;
#3754 = EDGE_CURVE ( 'NONE', #10886, #4817, #8133, .T. ) ;
#3755 = CARTESIAN_POINT ( 'NONE',  ( -10.68655108903816142, 8.641875097208238543, 101.0000000000000000 ) ) ;
#3756 = CARTESIAN_POINT ( 'NONE',  ( -49.99999999999999289, 43.89999999999999858, -16.24598481164531449 ) ) ;
#3757 = CARTESIAN_POINT ( 'NONE',  ( -49.86468353124999453, 41.75937500034139305, -16.20201782572375393 ) ) ;
#3758 = VERTEX_POINT ( 'NONE', #4397 ) ;
#3759 =( NAMED_UNIT ( * ) SI_UNIT ( $, .STERADIAN. ) SOLID_ANGLE_UNIT ( ) );
#3760 = ORIENTED_EDGE ( 'NONE', *, *, #14987, .T. ) ;
#3761 = CARTESIAN_POINT ( 'NONE',  ( 0.000000000000000000, 282.0000000000000000, 0.000000000000000000 ) ) ;
#3762 = CARTESIAN_POINT ( 'NONE',  ( -30.81806926056963292, 27.55937500034139376, -42.41743335407647209 ) ) ;
#3763 = CARTESIAN_POINT ( 'NONE',  ( -30.27664397204056712, 25.00000000000000355, -26.14048258526036150 ) ) ;
#3765 = EDGE_CURVE ( 'NONE', #5291, #10026, #10627, .T. ) ;
#3764 = CARTESIAN_POINT ( 'NONE',  ( -17.50000000000000000, 22.50000000000000000, 94.42467108177066848 ) ) ;
#3766 = CARTESIAN_POINT ( 'NONE',  ( 48.32661496269174961, 25.00000000000000000, -12.28922088333727558 ) ) ;
#3767 = CARTESIAN_POINT ( 'NONE',  ( 30.81806926056964002, 32.62187500034140442, 42.41743335407646498 ) ) ;
#3768 = CARTESIAN_POINT ( 'NONE',  ( 2.600676159226421000E-13, 33.49999999999999289, -49.99999999999999289 ) ) ;
#3769 = CARTESIAN_POINT ( 'NONE',  ( 49.86468353124999453, 25.02187500034139589, -16.20201782572376459 ) ) ;
#3770 = CARTESIAN_POINT ( 'NONE',  ( 30.81806926056962936, 23.15937500034139518, -42.41743335407646498 ) ) ;
#3771 = DIRECTION ( 'NONE',  ( 0.000000000000000000, 0.000000000000000000, 1.000000000000000000 ) ) ;
#3772 = CARTESIAN_POINT ( 'NONE',  ( 49.86468353125001585, 34.82187500034139305, 16.20201782572375038 ) ) ;
#3773 = DIRECTION ( 'NONE',  ( -0.7071067811865465735, 0.7071067811865484609, 1.635512977795596615E-16 ) ) ;
#3774 = CARTESIAN_POINT ( 'NONE',  ( -50.00000000000000000, 30.00000000000000355, 0.000000000000000000 ) ) ;
#3775 = CARTESIAN_POINT ( 'NONE',  ( 49.86468353125000164, 40.85937500034139447, -6.106662507704105588E-15 ) ) ;
#3776 = CARTESIAN_POINT ( 'NONE',  ( 30.81806926056964002, 32.62187500034140442, 42.41743335407647209 ) ) ;
#3777 = CARTESIAN_POINT ( 'NONE',  ( -15.45084971874736368, 42.39999999999999858, 47.55282581475768211 ) ) ;
#3778 = ORIENTED_EDGE ( 'NONE', *, *, #4233, .F. ) ;
#3779 = EDGE_CURVE ( 'NONE', #1788, #8741, #3220, .T. ) ;
#3780 = CARTESIAN_POINT ( 'NONE',  ( -3.210462471511496205E-15, 35.35937500034140157, -52.43083105670540789 ) ) ;
#3781 = ORIENTED_EDGE ( 'NONE', *, *, #8775, .T. ) ;
#3782 = ORIENTED_EDGE ( 'NONE', *, *, #2358, .T. ) ;
#3783 = CARTESIAN_POINT ( 'NONE',  ( 20.06446087900059894, 286.3455096218831386, -7.532230439496852448 ) ) ;
#3784 = CARTESIAN_POINT ( 'NONE',  ( 15.40903463028481113, 47.25937500034140015, -47.42413220539094709 ) ) ;
#3785 = DIRECTION ( 'NONE',  ( -0.2079116908177665313, 0.9781476007338041345, 0.000000000000000000 ) ) ;
#3786 = CARTESIAN_POINT ( 'NONE',  ( -49.86468353125000164, 21.92187500034139802, 0.000000000000000000 ) ) ;
#3787 = CARTESIAN_POINT ( 'NONE',  ( -2.939893647802529930, 6.264020653511205516, 102.0000000000000142 ) ) ;
#3788 = EDGE_CURVE ( 'NONE', #4733, #10001, #1884, .T. ) ;
#3789 = CARTESIAN_POINT ( 'NONE',  ( -40.34137639590981905, 39.72187500034139873, -29.30972558990011478 ) ) ;
#3790 = CARTESIAN_POINT ( 'NONE',  ( -7.919222016226804328, 26.22999571913594963, 50.00000000000000000 ) ) ;
#3791 = CARTESIAN_POINT ( 'NONE',  ( 50.00000000000000711, 48.90000000000000568, 16.24598481164530739 ) ) ;
#3792 = MECHANICAL_DESIGN_GEOMETRIC_PRESENTATION_REPRESENTATION (  '', ( #10950 ), #14656 ) ;
#3793 = ADVANCED_FACE ( 'NONE', ( #14281 ), #10711, .T. ) ;
#3794 = CARTESIAN_POINT ( 'NONE',  ( 50.00000000000000711, 28.68125000068279462, 16.24598481164530739 ) ) ;
#3795 = CARTESIAN_POINT ( 'NONE',  ( -49.86468353125000164, 47.92187500034139447, 0.000000000000000000 ) ) ;
#3796 = CARTESIAN_POINT ( 'NONE',  ( -3.210462471511496205E-15, 33.42187500034140157, -52.43083105670540789 ) ) ;
#3797 = CARTESIAN_POINT ( 'NONE',  ( 24.78626291527397285, 25.00000000000000355, 5.650101528493621572 ) ) ;
#3798 = DIRECTION ( 'NONE',  ( 0.000000000000000000, 0.000000000000000000, -1.000000000000000000 ) ) ;
#3799 = VERTEX_POINT ( 'NONE', #9307 ) ;
#3800 = VECTOR ( 'NONE', #5369, 1000.000000000000000 ) ;
#3801 = EDGE_LOOP ( 'NONE', ( #14574, #8800, #6894, #1206 ) ) ;
#3802 = CARTESIAN_POINT ( 'NONE',  ( 37.77664397204061686, 40.00000000000000711, 13.15010152849349900 ) ) ;
#3803 = CARTESIAN_POINT ( 'NONE',  ( 7.919222016226791006, 44.55125428154683931, 50.00000000000000711 ) ) ;
#3804 = DIRECTION ( 'NONE',  ( 0.000000000000000000, 0.000000000000000000, -1.000000000000000000 ) ) ;
#3805 = CARTESIAN_POINT ( 'NONE',  ( 0.000000000000000000, 51.99999999999999289, 0.000000000000000000 ) ) ;
#3806 = CARTESIAN_POINT ( 'NONE',  ( 49.86468353125001585, 32.75937500034140015, 16.20201782572375038 ) ) ;
#3807 = EDGE_CURVE ( 'NONE', #5010, #3492, #13281, .T. ) ;
#3808 = FILL_AREA_STYLE_COLOUR ( '', #5324 ) ;
#3809 = CARTESIAN_POINT ( 'NONE',  ( 15.40903463028481113, 45.32187500034140015, -47.42413220539094709 ) ) ;
#3810 = CARTESIAN_POINT ( 'NONE',  ( 0.000000000000000000, 22.50000000000000000, 102.0000000000000142 ) ) ;
#3811 = AXIS2_PLACEMENT_3D ( 'NONE', #12967, #1812, #6664 ) ;
#3812 = CARTESIAN_POINT ( 'NONE',  ( 1.102175790126979847E-14, 92.00000000000001421, 14.08089297201389201 ) ) ;
#3813 = DIRECTION ( 'NONE',  ( 0.000000000000000000, 0.000000000000000000, 1.000000000000000000 ) ) ;
#3814 = ORIENTED_EDGE ( 'NONE', *, *, #3363, .F. ) ;
#3815 = CARTESIAN_POINT ( 'NONE',  ( 9.631387414534489405E-15, 24.35937500034139802, 52.43083105670540789 ) ) ;
#3816 = ORIENTED_EDGE ( 'NONE', *, *, #15445, .F. ) ;
#3817 = DIRECTION ( 'NONE',  ( -0.000000000000000000, -1.000000000000000000, -0.000000000000000000 ) ) ;
#3818 = EDGE_LOOP ( 'NONE', ( #11485, #6594 ) ) ;
#3819 = VERTEX_POINT ( 'NONE', #13360 ) ;
#3820 = EDGE_CURVE ( 'NONE', #7211, #9602, #6812, .T. ) ;
#3821 = CARTESIAN_POINT ( 'NONE',  ( 50.00000000000000711, 34.68125000068279462, 16.24598481164530739 ) ) ;
#3822 = DIRECTION ( 'NONE',  ( 0.000000000000000000, 0.000000000000000000, 1.000000000000000000 ) ) ;
#3823 = VECTOR ( 'NONE', #5344, 1000.000000000000000 ) ;
#3824 = PRESENTATION_STYLE_ASSIGNMENT (( #9228 ) ) ;
#3825 = CARTESIAN_POINT ( 'NONE',  ( -7.499999999999998224, 25.00000000000000355, -24.29058411375428150 ) ) ;
#3826 = DIRECTION ( 'NONE',  ( 0.000000000000000000, 1.000000000000000000, 0.000000000000000000 ) ) ;
#3827 = DIRECTION ( 'NONE',  ( -0.2079116908177665590, 0.9781476007338041345, 0.000000000000000000 ) ) ;
#3828 = CARTESIAN_POINT ( 'NONE',  ( -45.00000000000000000, 262.0000000000000000, 10.00000000000000178 ) ) ;
#3829 = DIRECTION ( 'NONE',  ( -0.000000000000000000, 1.000000000000000000, -0.000000000000000000 ) ) ;
#3830 = CARTESIAN_POINT ( 'NONE',  ( 0.5000000000000000000, 247.0000000000000284, 49.99999999999999289 ) ) ;
#3831 = CARTESIAN_POINT ( 'NONE',  ( 50.00000000000000711, 44.68125000068278752, 16.24598481164530739 ) ) ;
#3832 = CARTESIAN_POINT ( 'NONE',  ( 50.00000000000000711, 44.68125000068278752, 16.24598481164530739 ) ) ;
#3833 = CARTESIAN_POINT ( 'NONE',  ( -50.00000000000000000, 24.00000000000000000, 0.000000000000000000 ) ) ;
#3834 = CARTESIAN_POINT ( 'NONE',  ( -20.00000000000000355, 307.0000000000000568, 0.000000000000000000 ) ) ;
#3835 = ORIENTED_EDGE ( 'NONE', *, *, #3779, .T. ) ;
#3836 = AXIS2_PLACEMENT_3D ( 'NONE', #6300, #9197, #11445 ) ;
#3837 = CARTESIAN_POINT ( 'NONE',  ( 49.86468353124999453, 40.95937500034140299, -16.20201782572376459 ) ) ;
#3838 = ORIENTED_EDGE ( 'NONE', *, *, #3607, .T. ) ;
#3839 = CARTESIAN_POINT ( 'NONE',  ( 5.510910596163089556E-15, 217.0000000000000284, -45.00000000000000000 ) ) ;
#3841 = CARTESIAN_POINT ( 'NONE',  ( 9.631387414534489405E-15, 26.35937500034140157, 52.43083105670540789 ) ) ;
#3840 =( BOUNDED_CURVE ( )  B_SPLINE_CURVE ( 2, ( #5636, #4553, #4475, #13110, #4309, #1952, #9453, #3212, #1801, #2969, #15853, #13197, #8037 ),
 .UNSPECIFIED., .F., .F. ) 
 B_SPLINE_CURVE_WITH_KNOTS ( ( 3, 2, 2, 2, 2, 2, 3 ),
 ( 0.1166666666666666685, 0.1199999999999999956, 0.1266666666666666774, 0.1333333333333333315, 0.1400000000000000133, 0.1466666666666666674, 0.1499999999999999944 ),
 .UNSPECIFIED. ) 
 CURVE ( )  GEOMETRIC_REPRESENTATION_ITEM ( )  RATIONAL_B_SPLINE_CURVE ( ( 0.9755282581475768211, 0.9755282581475768211, 1.000000000000000000, 0.9510565162951535312, 1.000000000000000000, 0.9510565162951535312, 1.000000000000000000, 0.9510565162951535312, 1.000000000000000000, 0.9510565162951535312, 1.000000000000000000, 0.9755282581475768211, 0.9755282581475768211 ) ) 
 REPRESENTATION_ITEM ( '' )  );
#3842 = VERTEX_POINT ( 'NONE', #1961 ) ;
#3843 = CARTESIAN_POINT ( 'NONE',  ( 40.45084971874737079, 27.20000000000000284, -29.38926261462366440 ) ) ;
#3844 = FACE_OUTER_BOUND ( 'NONE', #1249, .T. ) ;
#3845 = CARTESIAN_POINT ( 'NONE',  ( 48.28553921371819513, 25.00000000000000000, -12.45074877219152576 ) ) ;
#3846 = CARTESIAN_POINT ( 'NONE',  ( 40.34137639590981905, 32.72187500034139873, 29.30972558990010768 ) ) ;
#3847 = CIRCLE ( 'NONE', #13133, 50.00000000000000000 ) ;
#3848 = CARTESIAN_POINT ( 'NONE',  ( 7.919222016226940219, 31.22999571913595673, -49.99999999999996447 ) ) ;
#3849 = CARTESIAN_POINT ( 'NONE',  ( 30.81806926056964002, 24.55937500034139376, 42.41743335407646498 ) ) ;
#3850 = CARTESIAN_POINT ( 'NONE',  ( 9.735664389687646693E-15, 272.0000000000000000, 79.49773270518484480 ) ) ;
#3851 = CARTESIAN_POINT ( 'NONE',  ( -30.81806926056962226, 36.22187500034139163, 42.41743335407647209 ) ) ;
#3852 = DIRECTION ( 'NONE',  ( 1.000000000000000000, 1.784287003861858816E-14, 0.000000000000000000 ) ) ;
#3853 = CARTESIAN_POINT ( 'NONE',  ( 50.00000000000000000, 29.00000000000000000, -6.123233995736766085E-15 ) ) ;
#3854 = CARTESIAN_POINT ( 'NONE',  ( 49.86468353124999453, 38.95937500034139589, -16.20201782572376459 ) ) ;
#3855 = CARTESIAN_POINT ( 'NONE',  ( -15.40903463028481646, 29.52187500034139589, -47.42413220539093999 ) ) ;
#3856 = CARTESIAN_POINT ( 'NONE',  ( -15.45084971874737256, 47.60000000000000142, -47.55282581475767500 ) ) ;
#3857 = ORIENTED_EDGE ( 'NONE', *, *, #7088, .T. ) ;
#3858 = VERTEX_POINT ( 'NONE', #724 ) ;
#3859 = VECTOR ( 'NONE', #4778, 999.9999999999998863 ) ;
#3860 = CARTESIAN_POINT ( 'NONE',  ( 9.631387414534489405E-15, 34.35937500034140157, 52.43083105670540789 ) ) ;
#3861 = ORIENTED_EDGE ( 'NONE', *, *, #5945, .T. ) ;
#3862 = ORIENTED_EDGE ( 'NONE', *, *, #12206, .F. ) ;
#3863 = CARTESIAN_POINT ( 'NONE',  ( 30.00000000000000711, 282.0000000000000000, -12.50000000000000000 ) ) ;
#3864 = CARTESIAN_POINT ( 'NONE',  ( -15.40903463028480580, 48.25937500034140015, 47.42413220539094709 ) ) ;
#3865 = CARTESIAN_POINT ( 'NONE',  ( -49.93234176562499727, 49.96093750017070079, 0.000000000000000000 ) ) ;
#3866 = CARTESIAN_POINT ( 'NONE',  ( 30.81806926056962936, 21.22187500034139518, -42.41743335407647209 ) ) ;
#3867 = DIRECTION ( 'NONE',  ( -1.000000000000000000, 0.000000000000000000, 0.000000000000000000 ) ) ;
#3868 = CARTESIAN_POINT ( 'NONE',  ( -30.81806926056963292, 43.62187500034139020, -42.41743335407647209 ) ) ;
#3869 = DIRECTION ( 'NONE',  ( 1.000000000000000000, -0.000000000000000000, -0.000000000000000000 ) ) ;
#3870 = AXIS2_PLACEMENT_3D ( 'NONE', #13443, #1882, #6975 ) ;
#3871 = EDGE_CURVE ( 'NONE', #9378, #15183, #7852, .T. ) ;
#3872 = CARTESIAN_POINT ( 'NONE',  ( 50.00000000000000711, 44.90000000000000568, 16.24598481164530739 ) ) ;
#3873 = CARTESIAN_POINT ( 'NONE',  ( -40.45084971874737079, 25.98125000068279888, 29.38926261462367151 ) ) ;
#3874 = CARTESIAN_POINT ( 'NONE',  ( 4.539827090575156987, 39.41081929220959523, 92.94164601386977154 ) ) ;
#3875 = STYLED_ITEM ( 'NONE', ( #9556 ), #9194 ) ;
#3876 = CARTESIAN_POINT ( 'NONE',  ( 49.86468353125000164, 32.92187500034139447, -6.106662507704105588E-15 ) ) ;
#3877 = EDGE_CURVE ( 'NONE', #14668, #14510, #6823, .T. ) ;
#3878 = ADVANCED_FACE ( 'NONE', ( #13205, #10801 ), #4318, .T. ) ;
#3879 = ORIENTED_EDGE ( 'NONE', *, *, #10122, .F. ) ;
#3880 = CIRCLE ( 'NONE', #11851, 17.50000000000000000 ) ;
#3881 = VECTOR ( 'NONE', #6264, 1000.000000000000000 ) ;
#3882 = VERTEX_POINT ( 'NONE', #1809 ) ;
#3883 = PRODUCT_DEFINITION_FORMATION_WITH_SPECIFIED_SOURCE ( 'ANY', '', #8125, .NOT_KNOWN. ) ;
#3884 = DIRECTION ( 'NONE',  ( -0.9510565162951544194, 0.3090169943749449533, 0.000000000000000000 ) ) ;
#3885 = DIRECTION ( 'NONE',  ( 0.000000000000000000, 0.000000000000000000, 1.000000000000000000 ) ) ;
#3886 = PLANE ( 'NONE',  #668 ) ;
#3887 = DIRECTION ( 'NONE',  ( 0.000000000000000000, 0.000000000000000000, 1.000000000000000000 ) ) ;
#3888 = CARTESIAN_POINT ( 'NONE',  ( 30.81806926056964002, 28.55937500034139731, 42.41743335407647209 ) ) ;
#3889 = CARTESIAN_POINT ( 'NONE',  ( 0.000000000000000000, 273.6527036446661896, 89.78914894885470233 ) ) ;
#3890 = CARTESIAN_POINT ( 'NONE',  ( -3.210462471511496205E-15, 47.42187500034138736, -52.43083105670540789 ) ) ;
#3891 = VECTOR ( 'NONE', #11737, 1000.000000000000000 ) ;
#3892 = SURFACE_STYLE_FILL_AREA ( #1301 ) ;
#3893 = CIRCLE ( 'NONE', #10789, 2.000000000000001776 ) ;
#3895 = DIRECTION ( 'NONE',  ( 0.4067366430757888285, 0.9135454576426059736, 0.000000000000000000 ) ) ;
#3894 = VECTOR ( 'NONE', #5023, 1000.000000000000000 ) ;
#3896 = AXIS2_PLACEMENT_3D ( 'NONE', #12478, #15963, #14700 ) ;
#3897 = DIRECTION ( 'NONE',  ( 0.5000000000000039968, -0.8660254037844363761, 0.000000000000000000 ) ) ;
#3898 = CARTESIAN_POINT ( 'NONE',  ( 6.661118525004998681, 38.69041383028350367, 101.0000000000000000 ) ) ;
#3899 = ORIENTED_EDGE ( 'NONE', *, *, #14634, .F. ) ;
#3900 = CARTESIAN_POINT ( 'NONE',  ( -49.86468353125000164, 49.92187500034140157, 0.000000000000000000 ) ) ;
#3901 = VERTEX_POINT ( 'NONE', #12116 ) ;
#3902 = CARTESIAN_POINT ( 'NONE',  ( -30.90169943749474513, 45.48125000068279178, -42.53254041760200721 ) ) ;
#3903 = ORIENTED_EDGE ( 'NONE', *, *, #15238, .F. ) ;
#3904 = VERTEX_POINT ( 'NONE', #15939 ) ;
#3905 = CARTESIAN_POINT ( 'NONE',  ( 40.45084971874737079, 34.98125000068279888, -29.38926261462366440 ) ) ;
#3906 = CARTESIAN_POINT ( 'NONE',  ( 30.00000000000000355, 282.0000000000000000, 6.938893903907227589E-15 ) ) ;
#3907 = VECTOR ( 'NONE', #6345, 1000.000000000000000 ) ;
#3908 = CARTESIAN_POINT ( 'NONE',  ( 50.00000000000000711, 28.89999999999999858, 16.24598481164530739 ) ) ;
#3909 = LINE ( 'NONE', #10142, #10092 ) ;
#3910 = CARTESIAN_POINT ( 'NONE',  ( 30.81806926056962936, 49.15937500034138452, -42.41743335407647209 ) ) ;
#3911 = LINE ( 'NONE', #2654, #15023 ) ;
#3912 = CARTESIAN_POINT ( 'NONE',  ( -6.668400408272873429E-15, 49.28125000068279604, -50.00000000000000000 ) ) ;
#3913 = CARTESIAN_POINT ( 'NONE',  ( 40.45084971874737789, 24.58125000068280031, 29.38926261462365375 ) ) ;
#3914 = CARTESIAN_POINT ( 'NONE',  ( 0.000000000000000000, 279.6527036446661327, 90.84711083310548929 ) ) ;
#3915 = CARTESIAN_POINT ( 'NONE',  ( 30.90169943749474157, 43.08125000068280031, -42.53254041760200721 ) ) ;
#3916 = CARTESIAN_POINT ( 'NONE',  ( 7.919222016226791006, 44.33250428222964246, 50.00000000000000711 ) ) ;
#3917 = AXIS2_PLACEMENT_3D ( 'NONE', #1404, #2492, #2580 ) ;
#3918 = LINE ( 'NONE', #9070, #11352 ) ;
#3919 = ORIENTED_EDGE ( 'NONE', *, *, #3118, .F. ) ;
#3920 = CARTESIAN_POINT ( 'NONE',  ( 15.40903463028482356, 44.45937500034139589, 47.42413220539093999 ) ) ;
#3921 = ORIENTED_EDGE ( 'NONE', *, *, #4905, .F. ) ;
#3922 = DIRECTION ( 'NONE',  ( -1.000000000000000000, 0.000000000000000000, 0.000000000000000000 ) ) ;
#3923 = CARTESIAN_POINT ( 'NONE',  ( 45.58196769024076644, 258.6644603543468861, 10.00000000000000178 ) ) ;
#3924 = CARTESIAN_POINT ( 'NONE',  ( -15.40903463028481646, 29.45937500034139589, -47.42413220539093999 ) ) ;
#3925 = ORIENTED_EDGE ( 'NONE', *, *, #12330, .F. ) ;
#3926 = EDGE_CURVE ( 'NONE', #2810, #15172, #9719, .T. ) ;
#3927 = CARTESIAN_POINT ( 'NONE',  ( 0.000000000000000000, 267.0000000000000000, 0.000000000000000000 ) ) ;
#3928 = CARTESIAN_POINT ( 'NONE',  ( -8.798974116419094216, 37.67024782698770480, 92.94692907539341320 ) ) ;
#3929 = CARTESIAN_POINT ( 'NONE',  ( 48.15826639445412383, 25.00000000000000000, -12.93428853971252401 ) ) ;
#3930 = CARTESIAN_POINT ( 'NONE',  ( 9.631387414534489405E-15, 32.42187500034139447, 52.43083105670540789 ) ) ;
#3931 = CARTESIAN_POINT ( 'NONE',  ( 30.90169943749473802, 31.08125000068280031, -42.53254041760200721 ) ) ;
#3932 = CARTESIAN_POINT ( 'NONE',  ( -40.34137639590981905, 25.65937500034139518, -29.30972558990011478 ) ) ;
#3933 = CARTESIAN_POINT ( 'NONE',  ( 40.45084971874737789, 42.80000000000000426, 29.38926261462365375 ) ) ;
#3934 = CARTESIAN_POINT ( 'NONE',  ( 49.86468353124999453, 31.02187500034139589, -16.20201782572376104 ) ) ;
#3935 = CARTESIAN_POINT ( 'NONE',  ( -17.50000000000000000, 22.50000000000000000, 80.00000000000000000 ) ) ;
#3936 = CARTESIAN_POINT ( 'NONE',  ( -30.90169943749474868, 31.70000000000000639, -42.53254041760200721 ) ) ;
#3937 = CARTESIAN_POINT ( 'NONE',  ( -40.34137639590981195, 40.05937500034140442, 29.30972558990012189 ) ) ;
#3938 = CARTESIAN_POINT ( 'NONE',  ( 49.86468353124999453, 33.02187500034139589, -16.20201782572376459 ) ) ;
#3939 = CARTESIAN_POINT ( 'NONE',  ( -50.00000000000000000, 42.00000000000000000, 0.000000000000000000 ) ) ;
#3940 = ORIENTED_EDGE ( 'NONE', *, *, #1818, .T. ) ;
#3941 =( BOUNDED_CURVE ( )  B_SPLINE_CURVE ( 3, ( #14660, #9537, #1868, #14581 ),
 .UNSPECIFIED., .F., .F. ) 
 B_SPLINE_CURVE_WITH_KNOTS ( ( 4, 4 ),
 ( 3.141592653589793116, 3.724683441357939273 ),
 .UNSPECIFIED. ) 
 CURVE ( )  GEOMETRIC_REPRESENTATION_ITEM ( )  RATIONAL_B_SPLINE_CURVE ( ( 1.000000000000000000, 0.9718672150731668680, 0.9718672150731668680, 1.000000000000000000 ) ) 
 REPRESENTATION_ITEM ( '' )  );
#3942 = PRODUCT_DEFINITION_CONTEXT ( 'detailed design', #12378, 'design' ) ;
#3943 = CARTESIAN_POINT ( 'NONE',  ( 30.81806926056962936, 33.15937500034139873, -42.41743335407646498 ) ) ;
#3944 = ORIENTED_EDGE ( 'NONE', *, *, #12365, .F. ) ;
#3945 = CARTESIAN_POINT ( 'NONE',  ( 25.48725218877856946, 284.2907069533056301, -7.987252188780951556 ) ) ;
#3946 = CARTESIAN_POINT ( 'NONE',  ( 9.631387414534489405E-15, 48.35937500034140157, 52.43083105670540789 ) ) ;
#3947 = DIRECTION ( 'NONE',  ( 0.000000000000000000, 0.7071067811865362485, 0.7071067811865587860 ) ) ;
#3948 = CARTESIAN_POINT ( 'NONE',  ( -15.40903463028480580, 22.32187500034139660, 47.42413220539094709 ) ) ;
#3949 = FACE_OUTER_BOUND ( 'NONE', #14803, .T. ) ;
#3950 = CARTESIAN_POINT ( 'NONE',  ( 49.86468353125000164, 40.92187500034139447, -6.106662507704105588E-15 ) ) ;
#3951 = CARTESIAN_POINT ( 'NONE',  ( -3.210462471511496205E-15, 39.35937500034138736, -52.43083105670540789 ) ) ;
#3952 = DIRECTION ( 'NONE',  ( -1.000000000000000000, 0.000000000000000000, 0.000000000000000000 ) ) ;
#3953 = CARTESIAN_POINT ( 'NONE',  ( -40.45084971874737079, 46.20000000000000284, 29.38926261462367151 ) ) ;
#3954 = CARTESIAN_POINT ( 'NONE',  ( 9.657523855033129090E-15, 26.28125000068279604, 52.57311121191334990 ) ) ;
#3955 = CARTESIAN_POINT ( 'NONE',  ( -50.00000000000000000, 35.78125000068280315, 0.000000000000000000 ) ) ;
#3956 = CARTESIAN_POINT ( 'NONE',  ( -40.34137639590981195, 34.12187500034139731, 29.30972558990012189 ) ) ;
#3957 = CARTESIAN_POINT ( 'NONE',  ( 2.500000000000000000, 245.0000000000000284, -49.99999999999999289 ) ) ;
#3958 = ORIENTED_EDGE ( 'NONE', *, *, #8349, .F. ) ;
#3959 = CARTESIAN_POINT ( 'NONE',  ( -49.99999999999999289, 39.68125000068280173, -16.24598481164531449 ) ) ;
#3960 = EDGE_CURVE ( 'NONE', #7907, #14575, #4485, .T. ) ;
#3961 = ORIENTED_EDGE ( 'NONE', *, *, #4074, .F. ) ;
#3962 = CARTESIAN_POINT ( 'NONE',  ( -30.90169943749474513, 31.70000000000000639, -42.53254041760200721 ) ) ;
#3963 = LINE ( 'NONE', #6387, #14456 ) ;
#3964 = CARTESIAN_POINT ( 'NONE',  ( -30.90169943749473447, 24.29999999999999716, 42.53254041760200721 ) ) ;
#3965 = CARTESIAN_POINT ( 'NONE',  ( 30.81806926056962936, 47.22187500034139873, -42.41743335407646498 ) ) ;
#3966 = CARTESIAN_POINT ( 'NONE',  ( -40.34137639590981195, 32.05937500034139731, 29.30972558990012189 ) ) ;
#3967 = EDGE_CURVE ( 'NONE', #15517, #6639, #5803, .T. ) ;
#3968 = PRODUCT_RELATED_PRODUCT_CATEGORY ( 'part', '', ( #2806 ) ) ;
#3969 = CYLINDRICAL_SURFACE ( 'NONE', #11673, 5.000000000000000888 ) ;
#3970 = CARTESIAN_POINT ( 'NONE',  ( 30.81806926056962936, 49.22187500034139873, -42.41743335407646498 ) ) ;
#3971 = AXIS2_PLACEMENT_3D ( 'NONE', #15884, #7241, #4507 ) ;
#3972 = DIRECTION ( 'NONE',  ( 0.000000000000000000, 0.000000000000000000, 1.000000000000000000 ) ) ;
#3973 = CARTESIAN_POINT ( 'NONE',  ( 0.000000000000000000, 193.4213562373095385, 0.000000000000000000 ) ) ;
#3974 = CARTESIAN_POINT ( 'NONE',  ( 0.000000000000000000, 272.0000000000000000, 0.000000000000000000 ) ) ;
#3975 = EDGE_CURVE ( 'NONE', #11191, #10619, #16224, .T. ) ;
#3976 = CARTESIAN_POINT ( 'NONE',  ( 50.00000000000000711, 28.68125000068279462, 16.24598481164530739 ) ) ;
#3977 = ORIENTED_EDGE ( 'NONE', *, *, #10152, .T. ) ;
#3978 = CARTESIAN_POINT ( 'NONE',  ( 40.34137639590981905, 46.72187500034139873, 29.30972558990010768 ) ) ;
#3979 = ORIENTED_EDGE ( 'NONE', *, *, #281, .T. ) ;
#3980 = CARTESIAN_POINT ( 'NONE',  ( -7.919222016226816763, 25.55125428154684641, -49.99999999999999289 ) ) ;
#3981 = VERTEX_POINT ( 'NONE', #12362 ) ;
#3982 = EDGE_LOOP ( 'NONE', ( #11827, #985 ) ) ;
#3983 = EDGE_CURVE ( 'NONE', #8741, #15936, #3158, .T. ) ;
#3984 = AXIS2_PLACEMENT_3D ( 'NONE', #10064, #11543, #6159 ) ;
#3985 = CARTESIAN_POINT ( 'NONE',  ( -7.394441145214675437, 28.48516834767043093, 101.0000000000000000 ) ) ;
#3986 = CARTESIAN_POINT ( 'NONE',  ( 0.000000000000000000, 22.50000000000000000, 102.0000000000000142 ) ) ;
#3987 = CARTESIAN_POINT ( 'NONE',  ( 40.45084971874737079, 29.19999999999999929, -29.38926261462366440 ) ) ;
#3988 = CARTESIAN_POINT ( 'NONE',  ( -40.45084971874737079, 22.19999999999999929, 29.38926261462367151 ) ) ;
#3989 = CARTESIAN_POINT ( 'NONE',  ( -49.86468353125000164, 47.85937500034139447, 0.000000000000000000 ) ) ;
#3990 = LINE ( 'NONE', #15196, #2823 ) ;
#3991 = CARTESIAN_POINT ( 'NONE',  ( -15.45084971874736368, 26.18125000068280173, 47.55282581475768211 ) ) ;
#3992 = DIRECTION ( 'NONE',  ( 0.000000000000000000, 0.000000000000000000, -1.000000000000000000 ) ) ;
#3993 =( NAMED_UNIT ( * ) SI_UNIT ( $, .STERADIAN. ) SOLID_ANGLE_UNIT ( ) );
#3994 = CARTESIAN_POINT ( 'NONE',  ( 16.48898053797764973, 28.38332565970932819, 101.0000000000000000 ) ) ;
#3995 = CARTESIAN_POINT ( 'NONE',  ( -15.45084971874736368, 38.18125000068280173, 47.55282581475768211 ) ) ;
#3996 = CARTESIAN_POINT ( 'NONE',  ( 13.33959974903368995, 33.83821319854147447, 102.0000000000000142 ) ) ;
#3997 = ADVANCED_FACE ( 'NONE', ( #3558 ), #4899, .T. ) ;
#3998 = CARTESIAN_POINT ( 'NONE',  ( -40.45084971874737079, 20.20000000000000284, 29.38926261462367151 ) ) ;
#3999 = DIRECTION ( 'NONE',  ( 0.000000000000000000, 0.000000000000000000, -1.000000000000000000 ) ) ;
#4000 = ORIENTED_EDGE ( 'NONE', *, *, #5282, .T. ) ;
#4001 = CARTESIAN_POINT ( 'NONE',  ( 40.34137639590981905, 34.65937500034139873, 29.30972558990010768 ) ) ;
#4002 = VERTEX_POINT ( 'NONE', #13603 ) ;
#4003 = EDGE_CURVE ( 'NONE', #3234, #15272, #9864, .T. ) ;
#4004 = CARTESIAN_POINT ( 'NONE',  ( 9.366734789577542680E-15, 82.00000000000001421, -2.024759949320127682E-14 ) ) ;
#4005 = DIRECTION ( 'NONE',  ( -0.000000000000000000, 0.6143407043256620126, 0.7890408728378077718 ) ) ;
#4006 = CARTESIAN_POINT ( 'NONE',  ( -40.34137639590981195, 30.05937500034139731, 29.30972558990012189 ) ) ;
#4007 = ORIENTED_EDGE ( 'NONE', *, *, #10918, .T. ) ;
#4008 = PRODUCT_DEFINITION_SHAPE ( 'NONE', 'NONE',  #16474 ) ;
#4009 = DIRECTION ( 'NONE',  ( -0.000000000000000000, 1.000000000000000000, -0.000000000000000000 ) ) ;
#4010 = CARTESIAN_POINT ( 'NONE',  ( -15.97130229800533208, 29.67577800940753363, 93.41205153599007360 ) ) ;
#4011 = CARTESIAN_POINT ( 'NONE',  ( 46.31917516190732442, 25.00000000000000000, -18.46674513801128370 ) ) ;
#4012 = CARTESIAN_POINT ( 'NONE',  ( 49.86468353125000164, 36.92187500034140157, -6.106662507704105588E-15 ) ) ;
#4013 = CARTESIAN_POINT ( 'NONE',  ( 0.000000000000000000, 247.0000000000000284, 47.99999999999999289 ) ) ;
#4014 = CARTESIAN_POINT ( 'NONE',  ( -40.34137639590981195, 22.05937500034139731, 29.30972558990012189 ) ) ;
#4015 = CARTESIAN_POINT ( 'NONE',  ( -1.790468199911976477, 101.0808929720139417, 9.080892972013895559 ) ) ;
#4016 = ADVANCED_FACE ( 'NONE', ( #4742, #2208 ), #16268, .T. ) ;
#4017 = CARTESIAN_POINT ( 'NONE',  ( 49.86468353125001585, 28.82187500034139305, 16.20201782572375038 ) ) ;
#4018 = DIRECTION ( 'NONE',  ( 1.000000000000000000, 0.000000000000000000, 0.000000000000000000 ) ) ;
#4019 = CARTESIAN_POINT ( 'NONE',  ( 50.00000000000000000, 33.00000000000000000, -6.123233995736766085E-15 ) ) ;
#4020 = CARTESIAN_POINT ( 'NONE',  ( -30.81806926056963292, 33.55937500034138310, -42.41743335407647209 ) ) ;
#4021 = CARTESIAN_POINT ( 'NONE',  ( -3.210462471511496205E-15, 31.42187500034139447, -52.43083105670540789 ) ) ;
#4022 = ORIENTED_EDGE ( 'NONE', *, *, #711, .F. ) ;
#4023 = CARTESIAN_POINT ( 'NONE',  ( -49.86468353124999453, 33.75937500034140015, -16.20201782572375393 ) ) ;
#4024 = VERTEX_POINT ( 'NONE', #7305 ) ;
#4025 = ORIENTED_EDGE ( 'NONE', *, *, #15235, .T. ) ;
#4026 = CARTESIAN_POINT ( 'NONE',  ( 24.81239020281854835, 286.7275190727439735, -7.312390202817915075 ) ) ;
#4027 = CARTESIAN_POINT ( 'NONE',  ( -3.210462471511496205E-15, 45.35937500034139447, -52.43083105670540789 ) ) ;
#4028 = CARTESIAN_POINT ( 'NONE',  ( -37.77664397204053159, 40.00000000000000711, -13.15010152849376190 ) ) ;
#4029 = CARTESIAN_POINT ( 'NONE',  ( -15.40903463028480580, 26.32187500034140015, 47.42413220539094709 ) ) ;
#4030 = DIRECTION ( 'NONE',  ( -1.000000000000000000, 0.000000000000000000, 0.000000000000000000 ) ) ;
#4031 = CARTESIAN_POINT ( 'NONE',  ( -40.34137639590981905, 35.72187500034139163, -29.30972558990011478 ) ) ;
#4032 = CARTESIAN_POINT ( 'NONE',  ( -49.86468353124999453, 39.75937500034139305, -16.20201782572375393 ) ) ;
#4033 = CARTESIAN_POINT ( 'NONE',  ( -7.919222016226816763, 25.33250428222964246, -49.99999999999999289 ) ) ;
#4034 = CARTESIAN_POINT ( 'NONE',  ( 50.00000000000000000, 45.00000000000000711, -6.123233995736766085E-15 ) ) ;
#4035 = CARTESIAN_POINT ( 'NONE',  ( 30.90169943749475578, 22.48125000068279533, 42.53254041760200010 ) ) ;
#4036 = CARTESIAN_POINT ( 'NONE',  ( -49.86468353124999453, 49.82187500034140015, -16.20201782572375393 ) ) ;
#4037 =( BOUNDED_CURVE ( )  B_SPLINE_CURVE ( 2, ( #2176, #12248, #15909, #14814, #4533, #13572, #16160, #2099, #10923, #14899, #4871, #1015, #11006 ),
 .UNSPECIFIED., .F., .T. ) 
 B_SPLINE_CURVE_WITH_KNOTS ( ( 3, 2, 2, 2, 2, 2, 3 ),
 ( 0.4500000000000000111, 0.4533333333333333104, 0.4600000000000000200, 0.4666666666666666741, 0.4733333333333333282, 0.4799999999999999822, 0.4833333333333333370 ),
 .UNSPECIFIED. ) 
 CURVE ( )  GEOMETRIC_REPRESENTATION_ITEM ( )  RATIONAL_B_SPLINE_CURVE ( ( 0.9755282581475768211, 0.9755282581475770431, 1.000000000000000000, 0.9510565162951535312, 1.000000000000000000, 0.9510565162951535312, 1.000000000000000000, 0.9510565162951535312, 1.000000000000000000, 0.9510565162951535312, 1.000000000000000000, 0.9755282581475768211, 0.9755282581475768211 ) ) 
 REPRESENTATION_ITEM ( '' )  );
#4038 = CARTESIAN_POINT ( 'NONE',  ( -40.34137639590981905, 25.72187500034139518, -29.30972558990011478 ) ) ;
#4039 = EDGE_CURVE ( 'NONE', #16264, #14589, #15013, .T. ) ;
#4040 = CARTESIAN_POINT ( 'NONE',  ( -5.179451399590974781, 14.52044592729175321, 102.0000000000000142 ) ) ;
#4041 = EDGE_LOOP ( 'NONE', ( #10343, #14539, #2970, #8925, #7296 ) ) ;
#4042 = CARTESIAN_POINT ( 'NONE',  ( -40.45084971874737789, 35.58125000068279320, -29.38926261462365730 ) ) ;
#4043 = ORIENTED_EDGE ( 'NONE', *, *, #5569, .T. ) ;
#4044 = CARTESIAN_POINT ( 'NONE',  ( 41.80721665588484370, 98.34234248903790387, 5.000000000000000000 ) ) ;
#4045 = FACE_OUTER_BOUND ( 'NONE', #1941, .T. ) ;
#4046 = LINE ( 'NONE', #13847, #14738 ) ;
#4047 = CARTESIAN_POINT ( 'NONE',  ( 1.790468199911984692, 101.0808929720139560, -9.080892972013931086 ) ) ;
#4048 = CARTESIAN_POINT ( 'NONE',  ( 40.34137639590981195, 25.05937500034139376, -29.30972558990011834 ) ) ;
#4049 = CARTESIAN_POINT ( 'NONE',  ( 0.5000000000000000000, 39.65938208326293335, 101.3333374618097480 ) ) ;
#4050 = CARTESIAN_POINT ( 'NONE',  ( -0.5000000000000000000, 39.99999999999999289, 101.0000000000000000 ) ) ;
#4051 = CARTESIAN_POINT ( 'NONE',  ( -40.34137639590981195, 44.12187500034139731, 29.30972558990012189 ) ) ;
#4052 = DIRECTION ( 'NONE',  ( 1.000000000000000000, 0.000000000000000000, 0.000000000000000000 ) ) ;
#4053 = CYLINDRICAL_SURFACE ( 'NONE', #11528, 50.00000000000000000 ) ;
#4054 = CARTESIAN_POINT ( 'NONE',  ( -5.988468393965924008, 15.10823117958422301, 101.0000000000000000 ) ) ;
#4055 = VERTEX_POINT ( 'NONE', #8533 ) ;
#4056 = COLOUR_RGB ( '', 0.66274510, 0.83137255, 0.94901961) ;
#4057 = CARTESIAN_POINT ( 'NONE',  ( 15.40903463028481113, 47.32187500034140015, -47.42413220539094709 ) ) ;
#4058 = ORIENTED_EDGE ( 'NONE', *, *, #13590, .T. ) ;
#4059 = DIRECTION ( 'NONE',  ( -0.000000000000000000, 1.000000000000000000, -0.000000000000000000 ) ) ;
#4060 = ADVANCED_FACE ( 'NONE', ( #15347 ), #12612, .T. ) ;
#4061 = ORIENTED_EDGE ( 'NONE', *, *, #16244, .T. ) ;
#4062 = VERTEX_POINT ( 'NONE', #15176 ) ;
#4063 = FACE_OUTER_BOUND ( 'NONE', #6879, .T. ) ;
#4064 = DIRECTION ( 'NONE',  ( -0.6691306063588567943, -0.7431448254773955764, 0.000000000000000000 ) ) ;
#4065 = CARTESIAN_POINT ( 'NONE',  ( -3.219174618344376363E-15, 23.50000000000000000, -52.57311121191334990 ) ) ;
#4066 = CARTESIAN_POINT ( 'NONE',  ( 30.81806926056964002, 48.55937500034138310, 42.41743335407647209 ) ) ;
#4067 = DIRECTION ( 'NONE',  ( 0.4999999999999978351, 0.000000000000000000, -0.8660254037844399289 ) ) ;
#4068 = CARTESIAN_POINT ( 'NONE',  ( 7.919222016226693306, 24.33250428222964246, 50.00000000000003553 ) ) ;
#4069 = VECTOR ( 'NONE', #13568, 1000.000000000000114 ) ;
#4070 = CARTESIAN_POINT ( 'NONE',  ( 49.86468353125000164, 24.92187500034139802, -6.106662507704105588E-15 ) ) ;
#4071 = CARTESIAN_POINT ( 'NONE',  ( 8.446640517145639571E-15, 48.49999999999999289, 50.00000000000000000 ) ) ;
#4072 = CARTESIAN_POINT ( 'NONE',  ( -3.219174618344376363E-15, 41.28125000068280315, -52.57311121191334990 ) ) ;
#4073 = DIRECTION ( 'NONE',  ( 0.000000000000000000, 0.000000000000000000, 1.000000000000000000 ) ) ;
#4074 = EDGE_CURVE ( 'NONE', #11302, #8967, #409, .T. ) ;
#4075 = CARTESIAN_POINT ( 'NONE',  ( 50.00000000000000711, 20.68125000068279817, 16.24598481164530739 ) ) ;
#4076 = CARTESIAN_POINT ( 'NONE',  ( -6.386939227490606719, 38.07459704542236523, 101.6666710451724214 ) ) ;
#4077 = ORIENTED_EDGE ( 'NONE', *, *, #14561, .T. ) ;
#4078 = CARTESIAN_POINT ( 'NONE',  ( 30.81806926056962936, 37.15937500034139873, -42.41743335407647209 ) ) ;
#4079 = ADVANCED_FACE ( 'NONE', ( #7788 ), #3886, .F. ) ;
#4080 = VERTEX_POINT ( 'NONE', #10125 ) ;
#4081 = EDGE_CURVE ( 'NONE', #16202, #4152, #4046, .T. ) ;
#4082 = AXIS2_PLACEMENT_3D ( 'NONE', #7167, #13470, #5919 ) ;
#4083 = CARTESIAN_POINT ( 'NONE',  ( 15.45084971874737789, 42.60000000000000142, 47.55282581475767500 ) ) ;
#4084 = FACE_OUTER_BOUND ( 'NONE', #12288, .T. ) ;
#4085 = CARTESIAN_POINT ( 'NONE',  ( 49.86468353125001585, 20.75937500034140015, 16.20201782572375038 ) ) ;
#4086 = EDGE_LOOP ( 'NONE', ( #6865, #14652, #10573, #14800, #6150 ) ) ;
#4087 = EDGE_CURVE ( 'NONE', #495, #4982, #7343, .T. ) ;
#4088 = CARTESIAN_POINT ( 'NONE',  ( 50.00000000000000000, 27.00000000000000355, -6.123233995736766085E-15 ) ) ;
#4089 = CARTESIAN_POINT ( 'NONE',  ( -2.317185599438165467E-15, 40.00000000000004974, 92.94692077166139654 ) ) ;
#4090 = DIRECTION ( 'NONE',  ( -0.6691306063588671194, 0.7431448254773862505, 0.000000000000000000 ) ) ;
#4091 = CARTESIAN_POINT ( 'NONE',  ( 30.81806926056962936, 37.22187500034139163, -42.41743335407646498 ) ) ;
#4092 = CARTESIAN_POINT ( 'NONE',  ( -30.90169943749474513, 29.48125000068279888, -42.53254041760200721 ) ) ;
#4093 = CARTESIAN_POINT ( 'NONE',  ( 7.829870898593951800, 6.838588860456279228, 98.48475986922689174 ) ) ;
#4094 = CARTESIAN_POINT ( 'NONE',  ( -2.500000000000000000, 242.0000000000000284, 44.93050188902856945 ) ) ;
#4095 = CARTESIAN_POINT ( 'NONE',  ( 49.86468353125000164, 30.92187500034139802, -6.106662507704105588E-15 ) ) ;
#4096 = CARTESIAN_POINT ( 'NONE',  ( 2.500000000000000000, 242.0000000000000284, -44.93050188902856945 ) ) ;
#4097 = VECTOR ( 'NONE', #12557, 1000.000000000000000 ) ;
#4098 = CARTESIAN_POINT ( 'NONE',  ( 30.90169943749475578, 28.70000000000000284, 42.53254041760200010 ) ) ;
#4099 = CARTESIAN_POINT ( 'NONE',  ( 49.86468353125000164, 30.85937500034139802, -6.106662507704105588E-15 ) ) ;
#4100 = CARTESIAN_POINT ( 'NONE',  ( -3.210462471511496205E-15, 27.42187500034139092, -52.43083105670540789 ) ) ;
#4101 = CARTESIAN_POINT ( 'NONE',  ( -25.00000000000000711, 287.0000000000000568, -2.500000000000000444 ) ) ;
#4102 = VERTEX_POINT ( 'NONE', #7542 ) ;
#4103 =( REPRESENTATION_RELATIONSHIP ('NONE','NONE', #6178, #15095 ) REPRESENTATION_RELATIONSHIP_WITH_TRANSFORMATION ( #3131 )SHAPE_REPRESENTATION_RELATIONSHIP( ) );
#4104 =( BOUNDED_CURVE ( )  B_SPLINE_CURVE ( 2, ( #14112, #14035, #1395, #11542, #1483, #4156, #14195, #5338, #5088, #6580, #10141, #6404, #7649 ),
 .UNSPECIFIED., .F., .T. ) 
 B_SPLINE_CURVE_WITH_KNOTS ( ( 3, 2, 2, 2, 2, 2, 3 ),
 ( 0.7166666666666666741, 0.7199999999999999734, 0.7266666666666666829, 0.7333333333333332815, 0.7399999999999999911, 0.7466666666666667007, 0.7500000000000000000 ),
 .UNSPECIFIED. ) 
 CURVE ( )  GEOMETRIC_REPRESENTATION_ITEM ( )  RATIONAL_B_SPLINE_CURVE ( ( 0.9755282581475768211, 0.9755282581475768211, 1.000000000000000000, 0.9510565162951535312, 1.000000000000000000, 0.9510565162951535312, 1.000000000000000000, 0.9510565162951535312, 1.000000000000000000, 0.9510565162951535312, 1.000000000000000000, 0.9755282581475768211, 0.9755282581475768211 ) ) 
 REPRESENTATION_ITEM ( '' )  );
#4105 = CARTESIAN_POINT ( 'NONE',  ( -40.34137639590981195, 32.05937500034139731, 29.30972558990012189 ) ) ;
#4106 = ORIENTED_EDGE ( 'NONE', *, *, #3090, .F. ) ;
#4107 = EDGE_CURVE ( 'NONE', #8153, #12133, #8957, .T. ) ;
#4108 = CARTESIAN_POINT ( 'NONE',  ( 24.93825083353323535, 285.3724546740180017, -7.438250833534492124 ) ) ;
#4109 = CARTESIAN_POINT ( 'NONE',  ( 9.657523855033129090E-15, 20.28125000068279959, 52.57311121191334990 ) ) ;
#4110 = CIRCLE ( 'NONE', #15509, 82.49773270518484480 ) ;
#4111 = CARTESIAN_POINT ( 'NONE',  ( -30.90169943749473447, 38.29999999999999716, 42.53254041760200721 ) ) ;
#4112 = CARTESIAN_POINT ( 'NONE',  ( 28.38892170791706349, 282.2553694771637538, 9.277843415834380991 ) ) ;
#4113 = ADVANCED_FACE ( 'NONE', ( #1210 ), #10293, .F. ) ;
#4114 = CARTESIAN_POINT ( 'NONE',  ( -28.07127062163743503, 282.3184422169439927, 10.57127062163423759 ) ) ;
#4115 = CARTESIAN_POINT ( 'NONE',  ( 15.40903463028482356, 34.52187500034140299, 47.42413220539093999 ) ) ;
#4116 = CARTESIAN_POINT ( 'NONE',  ( 15.40903463028481113, 43.25937500034139305, -47.42413220539094709 ) ) ;
#4117 = CARTESIAN_POINT ( 'NONE',  ( -9.681523229999493552, 8.323875655254827421, 101.3333374614808662 ) ) ;
#4118 = CARTESIAN_POINT ( 'NONE',  ( 40.45084971874737079, 41.20000000000000284, -29.38926261462366440 ) ) ;
#4119 = CARTESIAN_POINT ( 'NONE',  ( 15.45084971874737789, 24.38125000068279746, 47.55282581475767500 ) ) ;
#4120 = CARTESIAN_POINT ( 'NONE',  ( 17.50000000000001421, 23.63086963147864239, 94.22187259348842758 ) ) ;
#4121 = STYLED_ITEM ( 'NONE', ( #1982 ), #8848 ) ;
#4122 = CARTESIAN_POINT ( 'NONE',  ( 49.86468353125000164, 30.92187500034139802, -6.106662507704105588E-15 ) ) ;
#4123 = CARTESIAN_POINT ( 'NONE',  ( -15.45084971874737256, 27.60000000000000142, -47.55282581475767500 ) ) ;
#4124 = ORIENTED_EDGE ( 'NONE', *, *, #4192, .F. ) ;
#4125 = CARTESIAN_POINT ( 'NONE',  ( -49.99999999999999289, 39.88125000068279746, 16.24598481164533226 ) ) ;
#4126 = EDGE_LOOP ( 'NONE', ( #9510, #4963, #2897, #13373 ) ) ;
#4127 = CARTESIAN_POINT ( 'NONE',  ( 30.90169943749475223, 48.48125000068279888, 42.53254041760199300 ) ) ;
#4128 = DIRECTION ( 'NONE',  ( 0.000000000000000000, -0.000000000000000000, 1.000000000000000000 ) ) ;
#4130 = ADVANCED_FACE ( 'NONE', ( #14012 ), #4687, .T. ) ;
#4129 = AXIS2_PLACEMENT_3D ( 'NONE', #8131, #5337, #9306 ) ;
#4131 = CARTESIAN_POINT ( 'NONE',  ( 40.45084971874737079, 30.98125000068279888, -29.38926261462366440 ) ) ;
#4132 = CARTESIAN_POINT ( 'NONE',  ( -30.81806926056963292, 45.62187500034139020, -42.41743335407646498 ) ) ;
#4133 = ADVANCED_FACE ( 'NONE', ( #6467 ), #7626, .T. ) ;
#4134 = CARTESIAN_POINT ( 'NONE',  ( -40.34137639590981195, 22.05937500034139731, 29.30972558990012189 ) ) ;
#4135 = COLOUR_RGB ( '', 0.31764706, 0.68627451, 0.89019608) ;
#4136 = CARTESIAN_POINT ( 'NONE',  ( 0.000000000000000000, 193.4213562373095385, 0.000000000000000000 ) ) ;
#4137 =( BOUNDED_CURVE ( )  B_SPLINE_CURVE ( 2, ( #8645, #2332, #7413, #12483, #11240, #6832, #5504, #11882, #2734, #14439, #4166, #10644, #4071 ),
 .UNSPECIFIED., .F., .F. ) 
 B_SPLINE_CURVE_WITH_KNOTS ( ( 3, 2, 2, 2, 2, 2, 3 ),
 ( 0.01666666666666666644, 0.02000000000000000042, 0.02666666666666666838, 0.03333333333333333287, 0.04000000000000000083, 0.04666666666666666879, 0.05000000000000000278 ),
 .UNSPECIFIED. ) 
 CURVE ( )  GEOMETRIC_REPRESENTATION_ITEM ( )  RATIONAL_B_SPLINE_CURVE ( ( 0.9755282581475768211, 0.9755282581475768211, 1.000000000000000000, 0.9510565162951535312, 1.000000000000000000, 0.9510565162951535312, 1.000000000000000000, 0.9510565162951535312, 1.000000000000000000, 0.9510565162951535312, 1.000000000000000000, 0.9755282581475768211, 0.9755282581475768211 ) ) 
 REPRESENTATION_ITEM ( '' )  );
#4138 = CARTESIAN_POINT ( 'NONE',  ( -40.34137639590981195, 42.12187500034139731, 29.30972558990012189 ) ) ;
#4139 = CARTESIAN_POINT ( 'NONE',  ( 0.000000000000000000, 0.000000000000000000, 0.000000000000000000 ) ) ;
#4140 = CARTESIAN_POINT ( 'NONE',  ( 30.90169943749473802, 35.08125000068278609, -42.53254041760200721 ) ) ;
#4141 = CARTESIAN_POINT ( 'NONE',  ( -30.81806926056963292, 49.62187500034139020, -42.41743335407647209 ) ) ;
#4142 = DIRECTION ( 'NONE',  ( -0.4067366430757887175, -0.9135454576426059736, 0.000000000000000000 ) ) ;
#4143 = VECTOR ( 'NONE', #8941, 1000.000000000000000 ) ;
#4144 = VECTOR ( 'NONE', #1393, 1000.000000000000000 ) ;
#4145 = ORIENTED_EDGE ( 'NONE', *, *, #8705, .T. ) ;
#4146 = AXIS2_PLACEMENT_3D ( 'NONE', #3669, #8726, #11157 ) ;
#4147 = CARTESIAN_POINT ( 'NONE',  ( -40.34137639590981905, 47.72187500034139873, -29.30972558990011478 ) ) ;
#4148 = PRODUCT ( 'rubber clutch', 'rubber clutch', '', ( #6965 ) ) ;
#4149 = ORIENTED_EDGE ( 'NONE', *, *, #12874, .T. ) ;
#4150 = CARTESIAN_POINT ( 'NONE',  ( -2.445080149700054274E-14, 46.28125000068280315, 50.00000000000000000 ) ) ;
#4151 = EDGE_LOOP ( 'NONE', ( #12411, #16082, #9528, #12192 ) ) ;
#4152 = VERTEX_POINT ( 'NONE', #12697 ) ;
#4153 = AXIS2_PLACEMENT_3D ( 'NONE', #1129, #375, #8115 ) ;
#4154 = CARTESIAN_POINT ( 'NONE',  ( 6.123233995736766085E-15, 193.4213562373095385, 50.00000000000000000 ) ) ;
#4155 = DIRECTION ( 'NONE',  ( 1.000000000000000000, 0.000000000000000000, 1.734723475976807094E-17 ) ) ;
#4156 = CARTESIAN_POINT ( 'NONE',  ( -49.99999999999999289, 28.10000000000000497, 16.24598481164533226 ) ) ;
#4157 = CARTESIAN_POINT ( 'NONE',  ( -30.90169943749473802, 26.29999999999999716, 42.53254041760200721 ) ) ;
#4158 = CARTESIAN_POINT ( 'NONE',  ( -40.34137639590981195, 42.05937500034139731, 29.30972558990012189 ) ) ;
#4159 = AXIS2_PLACEMENT_3D ( 'NONE', #12148, #4587, #4429 ) ;
#4160 = VECTOR ( 'NONE', #6022, 999.9999999999998863 ) ;
#4161 = CARTESIAN_POINT ( 'NONE',  ( -49.99999999999999289, 31.68125000068279462, -16.24598481164531449 ) ) ;
#4162 = CARTESIAN_POINT ( 'NONE',  ( 1.010305842943185372E-14, 252.0000000000000000, -82.49773270518484480 ) ) ;
#4163 = VECTOR ( 'NONE', #3016, 1000.000000000000000 ) ;
#4164 = CARTESIAN_POINT ( 'NONE',  ( -2.445080149700054274E-14, 46.50000000000000711, 50.00000000000000000 ) ) ;
#4165 = FILL_AREA_STYLE ('',( #7895 ) ) ;
#4166 = CARTESIAN_POINT ( 'NONE',  ( 15.45084971874737789, 48.60000000000000142, 47.55282581475767500 ) ) ;
#4167 = CARTESIAN_POINT ( 'NONE',  ( 9.657523855033129090E-15, 42.28125000068278894, 52.57311121191334990 ) ) ;
#4168 = DIRECTION ( 'NONE',  ( 1.000000000000000000, 0.000000000000000000, 0.000000000000000000 ) ) ;
#4169 = CARTESIAN_POINT ( 'NONE',  ( 50.00000000000000711, 22.68125000068279817, 16.24598481164530739 ) ) ;
#4170 = CARTESIAN_POINT ( 'NONE',  ( 0.000000000000000000, 247.0000000000000284, 0.000000000000000000 ) ) ;
#4171 = ORIENTED_EDGE ( 'NONE', *, *, #9269, .F. ) ;
#4172 = CARTESIAN_POINT ( 'NONE',  ( 15.40903463028481113, 35.25937500034139305, -47.42413220539094709 ) ) ;
#4173 = ORIENTED_EDGE ( 'NONE', *, *, #9270, .T. ) ;
#4174 = AXIS2_PLACEMENT_3D ( 'NONE', #11695, #1151, #11160 ) ;
#4175 = VERTEX_POINT ( 'NONE', #11692 ) ;
#4176 = AXIS2_PLACEMENT_3D ( 'NONE', #14537, #3078, #15708 ) ;
#4177 = CARTESIAN_POINT ( 'NONE',  ( 50.00000000000000711, 48.68125000068279462, 16.24598481164530739 ) ) ;
#4178 = DIRECTION ( 'NONE',  ( 1.224646799147353207E-16, -1.000000000000000000, 0.000000000000000000 ) ) ;
#4179 = DIRECTION ( 'NONE',  ( -0.000000000000000000, -0.000000000000000000, -1.000000000000000000 ) ) ;
#4180 = EDGE_CURVE ( 'NONE', #7762, #12541, #12086, .T. ) ;
#4181 = ORIENTED_EDGE ( 'NONE', *, *, #1933, .T. ) ;
#4182 = DIRECTION ( 'NONE',  ( 0.000000000000000000, -1.000000000000000000, 0.000000000000000000 ) ) ;
#4183 = CARTESIAN_POINT ( 'NONE',  ( -2.547328955960238000E-13, 22.49999999999999645, 49.99999999999999289 ) ) ;
#4184 = DIRECTION ( 'NONE',  ( 0.000000000000000000, 0.000000000000000000, -1.000000000000000000 ) ) ;
#4185 = CARTESIAN_POINT ( 'NONE',  ( 15.40903463028482356, 28.52187500034139589, 47.42413220539093999 ) ) ;
#4186 = FACE_OUTER_BOUND ( 'NONE', #3801, .T. ) ;
#4187 = VECTOR ( 'NONE', #10570, 1000.000000000000000 ) ;
#4188 = CARTESIAN_POINT ( 'NONE',  ( 11.63664291089594371, 9.379540242982125520, 97.65878401859123414 ) ) ;
#4189 = CARTESIAN_POINT ( 'NONE',  ( -46.56218328577778465, 20.00000000000000355, 17.84593874833660720 ) ) ;
#4190 = CARTESIAN_POINT ( 'NONE',  ( -40.34137639590981905, 29.72187500034139518, -29.30972558990011478 ) ) ;
#4192 = EDGE_CURVE ( 'NONE', #15550, #14671, #8195, .T. ) ;
#4191 = AXIS2_PLACEMENT_3D ( 'NONE', #6061, #13601, #4740 ) ;
#4193 = CARTESIAN_POINT ( 'NONE',  ( -40.45084971874737079, 22.19999999999999929, 29.38926261462367151 ) ) ;
#4194 = CARTESIAN_POINT ( 'NONE',  ( 9.657523855033129090E-15, 34.50000000000000711, 52.57311121191334990 ) ) ;
#4195 = CARTESIAN_POINT ( 'NONE',  ( 30.81806926056962936, 33.15937500034139873, -42.41743335407647209 ) ) ;
#4196 = DIRECTION ( 'NONE',  ( -0.8660254037844433705, 0.000000000000000000, -0.4999999999999918399 ) ) ;
#4197 = ADVANCED_FACE ( 'NONE', ( #14093 ), #4987, .F. ) ;
#4198 = ORIENTED_EDGE ( 'NONE', *, *, #9133, .F. ) ;
#4199 = CARTESIAN_POINT ( 'NONE',  ( 30.81806926056964002, 32.55937500034139731, 42.41743335407646498 ) ) ;
#4200 = ORIENTED_EDGE ( 'NONE', *, *, #10371, .F. ) ;
#4201 = LINE ( 'NONE', #13245, #4420 ) ;
#4202 = CARTESIAN_POINT ( 'NONE',  ( -40.34137639590981905, 41.65937500034139873, -29.30972558990011478 ) ) ;
#4203 = EDGE_CURVE ( 'NONE', #13411, #7884, #10541, .T. ) ;
#4204 = CARTESIAN_POINT ( 'NONE',  ( -7.919222016226870942, 38.44874571845316069, 49.99999999999997158 ) ) ;
#4205 = CARTESIAN_POINT ( 'NONE',  ( 24.86904120090595072, 286.8604097559505703, 7.369041200904230315 ) ) ;
#4206 = DIRECTION ( 'NONE',  ( -3.469446951953613696E-16, 0.000000000000000000, -1.000000000000000000 ) ) ;
#4207 = CARTESIAN_POINT ( 'NONE',  ( 30.81806926056962936, 37.22187500034139873, -42.41743335407647209 ) ) ;
#4208 = CARTESIAN_POINT ( 'NONE',  ( 9.631387414534489405E-15, 34.35937500034140157, 52.43083105670540789 ) ) ;
#4209 = LINE ( 'NONE', #357, #7602 ) ;
#4210 = CARTESIAN_POINT ( 'NONE',  ( -15.45084971874736368, 42.39999999999999858, 47.55282581475768211 ) ) ;
#4211 = CARTESIAN_POINT ( 'NONE',  ( 40.34137639590981905, 48.65937500034139873, 29.30972558990010768 ) ) ;
#4212 = CARTESIAN_POINT ( 'NONE',  ( -30.81806926056962226, 46.22187500034139163, 42.41743335407647919 ) ) ;
#4213 = CARTESIAN_POINT ( 'NONE',  ( 30.81806926056962936, 25.22187500034139873, -42.41743335407647209 ) ) ;
#4214 = CARTESIAN_POINT ( 'NONE',  ( -30.90169943749474513, 27.48125000068279888, -42.53254041760200721 ) ) ;
#4215 = ORIENTED_EDGE ( 'NONE', *, *, #15916, .T. ) ;
#4217 = EDGE_CURVE ( 'NONE', #15703, #3201, #11579, .T. ) ;
#4216 = CARTESIAN_POINT ( 'NONE',  ( 15.45084971874736723, 29.18125000068279817, -47.55282581475768211 ) ) ;
#4218 = ORIENTED_EDGE ( 'NONE', *, *, #2226, .F. ) ;
#4219 = CARTESIAN_POINT ( 'NONE',  ( 50.00000000000000000, 48.78125000068279604, -6.123233995736766085E-15 ) ) ;
#4220 = DIRECTION ( 'NONE',  ( -5.069245582283711292E-17, -1.000000000000000000, 8.780190904559502465E-17 ) ) ;
#4221 = FACE_OUTER_BOUND ( 'NONE', #8527, .T. ) ;
#4222 = CARTESIAN_POINT ( 'NONE',  ( 9.631387414534489405E-15, 48.42187500034139447, 52.43083105670540789 ) ) ;
#4223 = CARTESIAN_POINT ( 'NONE',  ( 15.40903463028481113, 25.25937500034139660, -47.42413220539094709 ) ) ;
#4224 = CARTESIAN_POINT ( 'NONE',  ( -15.45084971874737256, 39.38125000068279746, -47.55282581475767500 ) ) ;
#4225 = CARTESIAN_POINT ( 'NONE',  ( -49.86468353124999453, 42.02187500034139589, 16.20201782572377169 ) ) ;
#4226 = SHAPE_DEFINITION_REPRESENTATION ( #11839, #15829 ) ;
#4227 = CARTESIAN_POINT ( 'NONE',  ( 49.99999999999999289, 34.88125000068280457, -16.24598481164532160 ) ) ;
#4228 = AXIS2_PLACEMENT_3D ( 'NONE', #11641, #7975, #15450 ) ;
#4229 = CARTESIAN_POINT ( 'NONE',  ( -30.81806926056963292, 47.62187500034139731, -42.41743335407647209 ) ) ;
#4230 = DIRECTION ( 'NONE',  ( 0.000000000000000000, 0.000000000000000000, -1.000000000000000000 ) ) ;
#4231 = ORIENTED_EDGE ( 'NONE', *, *, #14339, .T. ) ;
#4232 = CARTESIAN_POINT ( 'NONE',  ( 49.86468353125000164, 20.85937500034139802, -6.106662507704105588E-15 ) ) ;
#4233 = EDGE_CURVE ( 'NONE', #10949, #3473, #15054, .T. ) ;
#4234 = VERTEX_POINT ( 'NONE', #5390 ) ;
#4235 = CARTESIAN_POINT ( 'NONE',  ( -24.14213562373094746, 282.0000000000000000, 9.571067811865473729 ) ) ;
#4236 = EDGE_LOOP ( 'NONE', ( #16168, #5571, #11686, #5971 ) ) ;
#4237 = CARTESIAN_POINT ( 'NONE',  ( 0.5000000000000000000, 242.0000000000000284, 47.99999999999999289 ) ) ;
#4238 = CARTESIAN_POINT ( 'NONE',  ( -4.336808689942020818E-17, 312.0000000000000568, 2.500000000000001776 ) ) ;
#4239 =( BOUNDED_CURVE ( )  B_SPLINE_CURVE ( 3, ( #10556, #9303, #4235, #2973 ),
 .UNSPECIFIED., .F., .T. ) 
 B_SPLINE_CURVE_WITH_KNOTS ( ( 4, 4 ),
 ( 3.141592653589793116, 4.712388980384689674 ),
 .UNSPECIFIED. ) 
 CURVE ( )  GEOMETRIC_REPRESENTATION_ITEM ( )  RATIONAL_B_SPLINE_CURVE ( ( 1.000000000000000000, 0.8047378541243649375, 0.8047378541243649375, 1.000000000000000000 ) ) 
 REPRESENTATION_ITEM ( '' )  );
#4240 = DIRECTION ( 'NONE',  ( -0.000000000000000000, 1.000000000000000000, -0.000000000000000000 ) ) ;
#4241 = CARTESIAN_POINT ( 'NONE',  ( 30.90169943749475578, 26.70000000000000284, 42.53254041760200010 ) ) ;
#4242 = MECHANICAL_DESIGN_GEOMETRIC_PRESENTATION_REPRESENTATION (  '', ( #2096 ), #15381 ) ;
#4243 = CARTESIAN_POINT ( 'NONE',  ( 9.631387414534489405E-15, 46.35937500034139447, 52.43083105670540789 ) ) ;
#4244 = CARTESIAN_POINT ( 'NONE',  ( 1.036604930454412972E-14, 98.25246584726775723, 9.080892972013893782 ) ) ;
#4245 = DIRECTION ( 'NONE',  ( -0.000000000000000000, -1.000000000000000000, -0.000000000000000000 ) ) ;
#4246 = FACE_BOUND ( 'NONE', #10138, .T. ) ;
#4247 =( NAMED_UNIT ( * ) PLANE_ANGLE_UNIT ( ) SI_UNIT ( $, .RADIAN. ) );
#4248 = CARTESIAN_POINT ( 'NONE',  ( 19.99999999999999289, 312.0000000000000568, -7.500000000000000000 ) ) ;
#4249 = CARTESIAN_POINT ( 'NONE',  ( -49.99999999999999289, 33.68125000068278752, -16.24598481164531449 ) ) ;
#4250 = CARTESIAN_POINT ( 'NONE',  ( -30.90169943749473447, 38.08125000068280031, 42.53254041760200721 ) ) ;
#4251 = CARTESIAN_POINT ( 'NONE',  ( 40.45084971874737079, 20.98125000068279888, -29.38926261462366440 ) ) ;
#4252 = CARTESIAN_POINT ( 'NONE',  ( 5.510910596163090344E-15, 267.0000000000000000, 45.00000000000000711 ) ) ;
#4253 = EDGE_LOOP ( 'NONE', ( #4261, #3597, #8546, #5666 ) ) ;
#4254 = CARTESIAN_POINT ( 'NONE',  ( 49.86468353125000164, 34.85937500034140157, -6.106662507704105588E-15 ) ) ;
#4255 = VECTOR ( 'NONE', #2903, 1000.000000000000000 ) ;
#4256 = ORIENTED_EDGE ( 'NONE', *, *, #5027, .T. ) ;
#4257 = ORIENTED_EDGE ( 'NONE', *, *, #2451, .F. ) ;
#4258 = DIRECTION ( 'NONE',  ( 1.000000000000000000, 0.000000000000000000, 0.000000000000000000 ) ) ;
#4259 = DIRECTION ( 'NONE',  ( 0.000000000000000000, 1.000000000000000000, 0.000000000000000000 ) ) ;
#4260 = CARTESIAN_POINT ( 'NONE',  ( -3.210462471511496205E-15, 25.35937500034139802, -52.43083105670540789 ) ) ;
#4261 = ORIENTED_EDGE ( 'NONE', *, *, #307, .F. ) ;
#4262 = CARTESIAN_POINT ( 'NONE',  ( 49.99999999999999289, 35.10000000000000853, -16.24598481164532160 ) ) ;
#4263 = CARTESIAN_POINT ( 'NONE',  ( 0.000000000000000000, 193.4213562373095385, -47.00000000000000000 ) ) ;
#4264 = CARTESIAN_POINT ( 'NONE',  ( -15.40903463028481646, 27.52187500034139944, -47.42413220539093999 ) ) ;
#4265 = EDGE_CURVE ( 'NONE', #11932, #9758, #8276, .T. ) ;
#4266 = CARTESIAN_POINT ( 'NONE',  ( -49.99999999999999289, 37.68125000068279462, -16.24598481164531449 ) ) ;
#4267 = EDGE_CURVE ( 'NONE', #1767, #15481, #10774, .T. ) ;
#4268 = CARTESIAN_POINT ( 'NONE',  ( 10.76154604949448768, 8.652744724135910559, 97.88922921878788941 ) ) ;
#4269 = CARTESIAN_POINT ( 'NONE',  ( 4.350898428888834396E-14, 37.00000000000001421, 10.00000000000000355 ) ) ;
#4270 = CARTESIAN_POINT ( 'NONE',  ( 9.631387414534489405E-15, 28.42187500034139447, 52.43083105670540789 ) ) ;
#4271 = CARTESIAN_POINT ( 'NONE',  ( -7.919222016226688865, 21.55125428154684641, -50.00000000000003553 ) ) ;
#4272 = CARTESIAN_POINT ( 'NONE',  ( -30.90169943749473802, 34.29999999999998295, 42.53254041760200721 ) ) ;
#4273 = CARTESIAN_POINT ( 'NONE',  ( 40.34137639590981905, 30.65937500034139518, 29.30972558990010768 ) ) ;
#4274 = CARTESIAN_POINT ( 'NONE',  ( 13.33429048796497085, 33.83343271840296751, 101.0000000000000000 ) ) ;
#4275 = VERTEX_POINT ( 'NONE', #4379 ) ;
#4276 = CARTESIAN_POINT ( 'NONE',  ( 40.34137639590981905, 32.65937500034139873, 29.30972558990010768 ) ) ;
#4277 = ORIENTED_EDGE ( 'NONE', *, *, #5509, .T. ) ;
#4278 = EDGE_CURVE ( 'NONE', #9110, #7461, #10377, .T. ) ;
#4279 = PRODUCT_DEFINITION ( 'UNKNOWN', '', #15287, #5292 ) ;
#4280 = CARTESIAN_POINT ( 'NONE',  ( 2.500000000000000000, 242.0000000000000284, 47.99999999999999289 ) ) ;
#4281 = CARTESIAN_POINT ( 'NONE',  ( 9.631387414534489405E-15, 40.35937500034139447, 52.43083105670540789 ) ) ;
#4282 = CARTESIAN_POINT ( 'NONE',  ( -30.90169943749474513, 37.70000000000000284, -42.53254041760200721 ) ) ;
#4283 = FACE_BOUND ( 'NONE', #15883, .T. ) ;
#4284 = CARTESIAN_POINT ( 'NONE',  ( -25.03223043950028881, 286.3455096218659151, 2.564460878999443860 ) ) ;
#4285 = CARTESIAN_POINT ( 'NONE',  ( 15.40903463028482356, 38.52187500034139589, 47.42413220539093999 ) ) ;
#4286 = CARTESIAN_POINT ( 'NONE',  ( 30.81806926056964002, 38.55937500034139731, 42.41743335407646498 ) ) ;
#4287 = LINE ( 'NONE', #5619, #3620 ) ;
#4288 =( BOUNDED_SURFACE ( )  B_SPLINE_SURFACE ( 1, 2, ( 
 ( #15046, #12403, #7251, #15125, #10149, #8562, #8732, #16297, #4934, #8646, #2333, #6007, #6247, #13797, #16385, #2410, #2491, #7488, #12308, #11241, #910, #2160, #6168, #5096, #12558, #8811, #11075, #1076, #7414, #14962, #13716, #3750, #5019, #12484, #995, #16143, #11319, #1153, #13554, #7568, #9990, #9908, #6096, #4851, #10072, #13875, #12644, #3588, #1241, #11399, #4771, #3831, #15841, #15201, #16219, #9829, #14879, #3508, #13632, #2242, #11163, #12725, #7978, #14119, #6412, #1403, #1653, #3915, #1577, #13052, #15535, #6670, #1321, #5345, #11719, #4167, #318, #14289, #157, #9236, #15454, #7655, #15289, #5418, #11473, #4072, #2735, #2659, #5175, #10317, #7897, #6752, #2579, #2910, #11797, #12972, #10475, #12884, #396, #70, #5505, #10569, #1496, #10231, #15624, #8896, #13958, #8984, #14042, #11645, #7733, #12800, #6494, #11550, #5266, #15373, #3995, #9068, #7813, #6588, #239, #10397, #9144, #14202, #2827, #10645, #1034, #16006, #13127, #11026, #5583, #14367, #8447, #1734, #12441, #3545, #7292, #8522, #13591, #16094, #14915, #4729, #15698, #4325, #2285, #3380, #2196, #10941, #14747, #6131, #7377, #9393, #2986, #8598, #4632, #14440, #12349, #13510, #1816, #4811, #8145, #4249, #13212, #2116, #9696, #3064, #8055, #7205, #6833, #9788, #16181, #6908, #5879, #11883, #11962, #11121, #483, #12266, #789, #868, #5963, #14834, #3463, #950, #6049, #9862, #13673, #11201, #9314, #1111, #8857, #7527, #11362, #5063, #15247, #1194, #1286, #10115, #6458, #1366, #6293, #16429, #15088, #6540, #12689, #15165, #9944, #13916, #14999, #12846, #10036, #3794, #3715, #8945, #15335, #11516, #2534, #14003, #7454, #8773, #5221, #16253, #4976, #13836, #12520, #2622, #6377, #4888, #10280, #7615, #12599, #2449, #11441, #5139, #7697, #3954, #34, #10195, #3873, #6207, #3635, #113, #12768, #9028, #14083, #2699, #7775, #1449, #8691, #13758, #2370, #11278, #16337, #9106, #4119, #4368, #6630, #4290, #10684, #1782, #9353, #15417, #8016, #14404, #6875, #3026, #526, #2872, #11926, #1696, #10355, #1540, #8097, #4035, #6793, #5461, #5383, #7856, #13013, #10611, #15739, #5306, #5623, #9433, #15668, #13175, #14484, #3116, #8189, #12935, #11681, #13254, #14332, #1854, #11603, #10527, #201, #10439, #14165, #11841, #14252 ),
 ( #2781, #279, #15495, #1616, #448, #9191, #7939, #13091, #6708, #11760, #359, #15586, #4211, #5549, #2949, #9278, #2021, #12172, #15826, #16072, #7190, #9770, #2102, #12332, #13494, #601, #4615, #5695, #12005, #15989, #14902, #854, #2179, #10763, #10926, #772, #8344, #7115, #13575, #14817, #5862, #687, #4457, #9522, #3529, #6032, #3448, #11009, #4708, #12251, #933, #5948, #13330, #8266, #4794, #9678, #8510, #13405, #14728, #8582, #9850, #1934, #14569, #11105, #3360, #7025, #7276, #8431, #4536, #16164, #10848, #6950, #15912, #13656, #3193, #12080, #5781, #9599, #14646, #3275, #13985, #3613, #3701, #11185, #13743, #8919, #16240, #16412, #4874, #10018, #3775, #1097, #8677, #7439, #8758, #6190, #6115, #12505, #3937, #2356, #11346, #15072, #13820, #7509, #1268, #2432, #8834, #12581, #2603, #3854, #1178, #6273, #11265, #9010, #15149, #5045, #12427, #10098, #1020, #15317, #16322, #13898, #4957, #11424, #1346, #7679, #2513, #17, #9931, #7592, #12749, #2265, #12671, #6360, #14984, #5121, #6437, #10174, #11498, #95, #15224, #5198, #10254, #7363, #3010, #15721, #14389, #344, #6519, #1761, #11666, #5605, #510, #15649, #9089, #5288, #14146, #7756, #5367, #7920, #6863, #15477, #10423, #4020, #10670, #9170, #11578, #4195, #15401, #12826, #1599, #2853, #184, #6778, #14315, #428, #9259, #8081, #2934, #1429, #11741, #10339, #2682, #6693, #4352, #8001, #9339, #2762, #5443, #12996, #4099, #14228, #4273, #5532, #10506, #7838, #12912, #11821, #13075, #14066, #13153, #15565, #1678, #6611, #10593, #11910, #1522, #262, #666, #15973, #14630, #583, #16146, #9752, #12154, #12064, #13557, #7174, #913, #838, #4594, #5929, #13240, #8492, #3255, #6934, #1913, #2163, #4435, #2085, #7255, #16053, #12235, #1838, #5846, #10988, #4683, #14797, #3431, #5763, #12312, #9658, #8172, #15805, #6010, #11986, #14708, #8325, #3178, #5677, #10832, #8411, #11079, #3096, #9417, #14462, #13479, #10747, #9506, #14551, #8249, #13314, #7008, #15896, #755, #4520, #9585, #13390, #1998, #7095, #10909, #3339, #7418, #12407, #16300, #9992, #9833, #1157, #13962, #11403, #15050, #3512, #14882, #2494, #8814, #11244, #10075, #8650, #8565, #6251, #3592, #13635, #6339, #1325, #16222, #16389, #7491, #12561, #4938, #2337, #5099 ) ),
 .UNSPECIFIED., .F., .F., .F. ) 
 B_SPLINE_SURFACE_WITH_KNOTS ( ( 2, 2 ),
 ( 3, 2, 2, 2, 2, 2, 2, 2, 2, 2, 2, 2, 2, 2, 2, 2, 2, 2, 2, 2, 2, 2, 2, 2, 2, 2, 2, 2, 2, 2, 2, 2, 2, 2, 2, 2, 2, 2, 2, 2, 2, 2, 2, 2, 2, 2, 2, 2, 2, 2, 2, 2, 2, 2, 2, 2, 2, 2, 2, 2, 2, 2, 2, 2, 2, 2, 2, 2, 2, 2, 2, 2, 2, 2, 2, 2, 2, 2, 2, 2, 2, 2, 2, 2, 2, 2, 2, 2, 2, 2, 2, 2, 2, 2, 2, 2, 2, 2, 2, 2, 2, 2, 2, 2, 2, 2, 2, 2, 2, 2, 2, 2, 2, 2, 2, 2, 2, 2, 2, 2, 2, 2, 2, 2, 2, 2, 2, 2, 2, 2, 2, 2, 2, 2, 2, 2, 2, 2, 2, 2, 2, 2, 2, 2, 2, 2, 2, 2, 2, 2, 3 ),
 ( 0.000000000000000000, 1.000000000000000000 ),
 ( 0.000000000000000000, 0.006666666666666667095, 0.01333333333333333419, 0.02000000000000000042, 0.02666666666666666838, 0.03333333333333333287, 0.04000000000000000083, 0.04666666666666666879, 0.05333333333333333676, 0.05999999999999999778, 0.06666666666666666574, 0.07333333333333333370, 0.08000000000000000167, 0.08666666666666666963, 0.09333333333333333759, 0.1000000000000000056, 0.1066666666666666735, 0.1133333333333333276, 0.1199999999999999956, 0.1266666666666666774, 0.1333333333333333315, 0.1400000000000000133, 0.1466666666666666674, 0.1533333333333333215, 0.1600000000000000033, 0.1666666666666666574, 0.1733333333333333393, 0.1799999999999999933, 0.1866666666666666752, 0.1933333333333333293, 0.2000000000000000111, 0.2066666666666666652, 0.2133333333333333470, 0.2200000000000000011, 0.2266666666666666552, 0.2333333333333333370, 0.2399999999999999911, 0.2466666666666666730, 0.2533333333333333548, 0.2600000000000000089, 0.2666666666666666630, 0.2733333333333333171, 0.2800000000000000266, 0.2866666666666666807, 0.2933333333333333348, 0.2999999999999999889, 0.3066666666666666430, 0.3133333333333333526, 0.3200000000000000067, 0.3266666666666666607, 0.3333333333333333148, 0.3400000000000000244, 0.3466666666666666785, 0.3533333333333333326, 0.3599999999999999867, 0.3666666666666666408, 0.3733333333333333504, 0.3800000000000000044, 0.3866666666666666585, 0.3933333333333333126, 0.4000000000000000222, 0.4066666666666666763, 0.4133333333333333304, 0.4199999999999999845, 0.4266666666666666941, 0.4333333333333333481, 0.4400000000000000022, 0.4466666666666666563, 0.4533333333333333104, 0.4600000000000000200, 0.4666666666666666741, 0.4733333333333333282, 0.4799999999999999822, 0.4866666666666666918, 0.4933333333333333459, 0.5000000000000000000, 0.5066666666666667096, 0.5133333333333333082, 0.5200000000000000178, 0.5266666666666666163, 0.5333333333333333259, 0.5400000000000000355, 0.5466666666666666341, 0.5533333333333333437, 0.5600000000000000533, 0.5666666666666666519, 0.5733333333333333615, 0.5799999999999999600, 0.5866666666666666696, 0.5933333333333333792, 0.5999999999999999778, 0.6066666666666666874, 0.6133333333333332860, 0.6199999999999999956, 0.6266666666666667052, 0.6333333333333333037, 0.6400000000000000133, 0.6466666666666666119, 0.6533333333333333215, 0.6600000000000000311, 0.6666666666666666297, 0.6733333333333333393, 0.6800000000000000488, 0.6866666666666666474, 0.6933333333333333570, 0.6999999999999999556, 0.7066666666666666652, 0.7133333333333333748, 0.7199999999999999734, 0.7266666666666666829, 0.7333333333333332815, 0.7399999999999999911, 0.7466666666666667007, 0.7533333333333332993, 0.7600000000000000089, 0.7666666666666667185, 0.7733333333333333171, 0.7800000000000000266, 0.7866666666666666252, 0.7933333333333333348, 0.8000000000000000444, 0.8066666666666666430, 0.8133333333333333526, 0.8199999999999999512, 0.8266666666666666607, 0.8333333333333333703, 0.8399999999999999689, 0.8466666666666666785, 0.8533333333333333881, 0.8599999999999999867, 0.8666666666666666963, 0.8733333333333332948, 0.8800000000000000044, 0.8866666666666667140, 0.8933333333333333126, 0.9000000000000000222, 0.9066666666666666208, 0.9133333333333333304, 0.9200000000000000400, 0.9266666666666666385, 0.9333333333333333481, 0.9399999999999999467, 0.9466666666666666563, 0.9533333333333333659, 0.9599999999999999645, 0.9666666666666666741, 0.9733333333333333837, 0.9799999999999999822, 0.9866666666666666918, 0.9933333333333332904, 1.000000000000000000 ),
 .UNSPECIFIED. ) 
 GEOMETRIC_REPRESENTATION_ITEM ( )  RATIONAL_B_SPLINE_SURFACE ( (
 ( 1.000000000000000000, 0.9510565162951535312, 1.000000000000000000, 0.9510565162951535312, 1.000000000000000000, 0.9510565162951535312, 1.000000000000000000, 0.9510565162951535312, 1.000000000000000000, 0.9510565162951535312, 1.000000000000000000, 0.9510565162951535312, 1.000000000000000000, 0.9510565162951535312, 1.000000000000000000, 0.9510565162951535312, 1.000000000000000000, 0.9510565162951535312, 1.000000000000000000, 0.9510565162951535312, 1.000000000000000000, 0.9510565162951535312, 1.000000000000000000, 0.9510565162951535312, 1.000000000000000000, 0.9510565162951535312, 1.000000000000000000, 0.9510565162951535312, 1.000000000000000000, 0.9510565162951535312, 1.000000000000000000, 0.9510565162951535312, 1.000000000000000000, 0.9510565162951535312, 1.000000000000000000, 0.9510565162951535312, 1.000000000000000000, 0.9510565162951535312, 1.000000000000000000, 0.9510565162951535312, 1.000000000000000000, 0.9510565162951535312, 1.000000000000000000, 0.9510565162951535312, 1.000000000000000000, 0.9510565162951535312, 1.000000000000000000, 0.9510565162951535312, 1.000000000000000000, 0.9510565162951535312, 1.000000000000000000, 0.9510565162951535312, 1.000000000000000000, 0.9510565162951535312, 1.000000000000000000, 0.9510565162951535312, 1.000000000000000000, 0.9510565162951535312, 1.000000000000000000, 0.9510565162951535312, 1.000000000000000000, 0.9510565162951535312, 1.000000000000000000, 0.9510565162951535312, 1.000000000000000000, 0.9510565162951535312, 1.000000000000000000, 0.9510565162951535312, 1.000000000000000000, 0.9510565162951535312, 1.000000000000000000, 0.9510565162951535312, 1.000000000000000000, 0.9510565162951535312, 1.000000000000000000, 0.9510565162951535312, 1.000000000000000000, 0.9510565162951535312, 1.000000000000000000, 0.9510565162951535312, 1.000000000000000000, 0.9510565162951535312, 1.000000000000000000, 0.9510565162951535312, 1.000000000000000000, 0.9510565162951535312, 1.000000000000000000, 0.9510565162951535312, 1.000000000000000000, 0.9510565162951535312, 1.000000000000000000, 0.9510565162951535312, 1.000000000000000000, 0.9510565162951535312, 1.000000000000000000, 0.9510565162951535312, 1.000000000000000000, 0.9510565162951535312, 1.000000000000000000, 0.9510565162951535312, 1.000000000000000000, 0.9510565162951535312, 1.000000000000000000, 0.9510565162951535312, 1.000000000000000000, 0.9510565162951535312, 1.000000000000000000, 0.9510565162951535312, 1.000000000000000000, 0.9510565162951535312, 1.000000000000000000, 0.9510565162951535312, 1.000000000000000000, 0.9510565162951535312, 1.000000000000000000, 0.9510565162951535312, 1.000000000000000000, 0.9510565162951535312, 1.000000000000000000, 0.9510565162951535312, 1.000000000000000000, 0.9510565162951535312, 1.000000000000000000, 0.9510565162951535312, 1.000000000000000000, 0.9510565162951535312, 1.000000000000000000, 0.9510565162951535312, 1.000000000000000000, 0.9510565162951535312, 1.000000000000000000, 0.9510565162951535312, 1.000000000000000000, 0.9510565162951535312, 1.000000000000000000, 0.9510565162951535312, 1.000000000000000000, 0.9510565162951535312, 1.000000000000000000, 0.9510565162951535312, 1.000000000000000000, 0.9510565162951535312, 1.000000000000000000, 0.9510565162951535312, 1.000000000000000000, 0.9510565162951535312, 1.000000000000000000, 0.9510565162951535312, 1.000000000000000000, 0.9510565162951535312, 1.000000000000000000, 0.9510565162951535312, 1.000000000000000000, 0.9510565162951535312, 1.000000000000000000, 0.9510565162951535312, 1.000000000000000000, 0.9510565162951535312, 1.000000000000000000, 0.9510565162951535312, 1.000000000000000000, 0.9510565162951535312, 1.000000000000000000, 0.9510565162951535312, 1.000000000000000000, 0.9510565162951535312, 1.000000000000000000, 0.9510565162951535312, 1.000000000000000000, 0.9510565162951535312, 1.000000000000000000, 0.9510565162951535312, 1.000000000000000000, 0.9510565162951535312, 1.000000000000000000, 0.9510565162951535312, 1.000000000000000000, 0.9510565162951535312, 1.000000000000000000, 0.9510565162951535312, 1.000000000000000000, 0.9510565162951535312, 1.000000000000000000, 0.9510565162951535312, 1.000000000000000000, 0.9510565162951535312, 1.000000000000000000, 0.9510565162951535312, 1.000000000000000000, 0.9510565162951535312, 1.000000000000000000, 0.9510565162951535312, 1.000000000000000000, 0.9510565162951535312, 1.000000000000000000, 0.9510565162951535312, 1.000000000000000000, 0.9510565162951535312, 1.000000000000000000, 0.9510565162951535312, 1.000000000000000000, 0.9510565162951535312, 1.000000000000000000, 0.9510565162951535312, 1.000000000000000000, 0.9510565162951535312, 1.000000000000000000, 0.9510565162951535312, 1.000000000000000000, 0.9510565162951535312, 1.000000000000000000, 0.9510565162951535312, 1.000000000000000000, 0.9510565162951535312, 1.000000000000000000, 0.9510565162951535312, 1.000000000000000000, 0.9510565162951535312, 1.000000000000000000, 0.9510565162951535312, 1.000000000000000000, 0.9510565162951535312, 1.000000000000000000, 0.9510565162951535312, 1.000000000000000000, 0.9510565162951535312, 1.000000000000000000, 0.9510565162951535312, 1.000000000000000000, 0.9510565162951535312, 1.000000000000000000, 0.9510565162951535312, 1.000000000000000000, 0.9510565162951535312, 1.000000000000000000, 0.9510565162951535312, 1.000000000000000000, 0.9510565162951535312, 1.000000000000000000, 0.9510565162951535312, 1.000000000000000000, 0.9510565162951535312, 1.000000000000000000, 0.9510565162951535312, 1.000000000000000000, 0.9510565162951535312, 1.000000000000000000, 0.9510565162951535312, 1.000000000000000000, 0.9510565162951535312, 1.000000000000000000, 0.9510565162951535312, 1.000000000000000000, 0.9510565162951535312, 1.000000000000000000, 0.9510565162951535312, 1.000000000000000000, 0.9510565162951535312, 1.000000000000000000, 0.9510565162951535312, 1.000000000000000000, 0.9510565162951535312, 1.000000000000000000, 0.9510565162951535312, 1.000000000000000000, 0.9510565162951535312, 1.000000000000000000, 0.9510565162951535312, 1.000000000000000000, 0.9510565162951535312, 1.000000000000000000, 0.9510565162951535312, 1.000000000000000000, 0.9510565162951535312, 1.000000000000000000, 0.9510565162951535312, 1.000000000000000000, 0.9510565162951535312, 1.000000000000000000, 0.9510565162951535312, 1.000000000000000000, 0.9510565162951535312, 1.000000000000000000, 0.9510565162951535312, 1.000000000000000000, 0.9510565162951535312, 1.000000000000000000, 0.9510565162951535312, 1.000000000000000000, 0.9510565162951535312, 1.000000000000000000, 0.9510565162951535312, 1.000000000000000000, 0.9510565162951535312, 1.000000000000000000, 0.9510565162951535312, 1.000000000000000000, 0.9510565162951535312, 1.000000000000000000, 0.9510565162951535312, 1.000000000000000000),
 ( 1.000000000000000000, 0.9510565162951535312, 1.000000000000000000, 0.9510565162951535312, 1.000000000000000000, 0.9510565162951535312, 1.000000000000000000, 0.9510565162951535312, 1.000000000000000000, 0.9510565162951535312, 1.000000000000000000, 0.9510565162951535312, 1.000000000000000000, 0.9510565162951535312, 1.000000000000000000, 0.9510565162951535312, 1.000000000000000000, 0.9510565162951535312, 1.000000000000000000, 0.9510565162951535312, 1.000000000000000000, 0.9510565162951535312, 1.000000000000000000, 0.9510565162951535312, 1.000000000000000000, 0.9510565162951535312, 1.000000000000000000, 0.9510565162951535312, 1.000000000000000000, 0.9510565162951535312, 1.000000000000000000, 0.9510565162951535312, 1.000000000000000000, 0.9510565162951535312, 1.000000000000000000, 0.9510565162951535312, 1.000000000000000000, 0.9510565162951535312, 1.000000000000000000, 0.9510565162951535312, 1.000000000000000000, 0.9510565162951535312, 1.000000000000000000, 0.9510565162951535312, 1.000000000000000000, 0.9510565162951535312, 1.000000000000000000, 0.9510565162951535312, 1.000000000000000000, 0.9510565162951535312, 1.000000000000000000, 0.9510565162951535312, 1.000000000000000000, 0.9510565162951535312, 1.000000000000000000, 0.9510565162951535312, 1.000000000000000000, 0.9510565162951535312, 1.000000000000000000, 0.9510565162951535312, 1.000000000000000000, 0.9510565162951535312, 1.000000000000000000, 0.9510565162951535312, 1.000000000000000000, 0.9510565162951535312, 1.000000000000000000, 0.9510565162951535312, 1.000000000000000000, 0.9510565162951535312, 1.000000000000000000, 0.9510565162951535312, 1.000000000000000000, 0.9510565162951535312, 1.000000000000000000, 0.9510565162951535312, 1.000000000000000000, 0.9510565162951535312, 1.000000000000000000, 0.9510565162951535312, 1.000000000000000000, 0.9510565162951535312, 1.000000000000000000, 0.9510565162951535312, 1.000000000000000000, 0.9510565162951535312, 1.000000000000000000, 0.9510565162951535312, 1.000000000000000000, 0.9510565162951535312, 1.000000000000000000, 0.9510565162951535312, 1.000000000000000000, 0.9510565162951535312, 1.000000000000000000, 0.9510565162951535312, 1.000000000000000000, 0.9510565162951535312, 1.000000000000000000, 0.9510565162951535312, 1.000000000000000000, 0.9510565162951535312, 1.000000000000000000, 0.9510565162951535312, 1.000000000000000000, 0.9510565162951535312, 1.000000000000000000, 0.9510565162951535312, 1.000000000000000000, 0.9510565162951535312, 1.000000000000000000, 0.9510565162951535312, 1.000000000000000000, 0.9510565162951535312, 1.000000000000000000, 0.9510565162951535312, 1.000000000000000000, 0.9510565162951535312, 1.000000000000000000, 0.9510565162951535312, 1.000000000000000000, 0.9510565162951535312, 1.000000000000000000, 0.9510565162951535312, 1.000000000000000000, 0.9510565162951535312, 1.000000000000000000, 0.9510565162951535312, 1.000000000000000000, 0.9510565162951535312, 1.000000000000000000, 0.9510565162951535312, 1.000000000000000000, 0.9510565162951535312, 1.000000000000000000, 0.9510565162951535312, 1.000000000000000000, 0.9510565162951535312, 1.000000000000000000, 0.9510565162951535312, 1.000000000000000000, 0.9510565162951535312, 1.000000000000000000, 0.9510565162951535312, 1.000000000000000000, 0.9510565162951535312, 1.000000000000000000, 0.9510565162951535312, 1.000000000000000000, 0.9510565162951535312, 1.000000000000000000, 0.9510565162951535312, 1.000000000000000000, 0.9510565162951535312, 1.000000000000000000, 0.9510565162951535312, 1.000000000000000000, 0.9510565162951535312, 1.000000000000000000, 0.9510565162951535312, 1.000000000000000000, 0.9510565162951535312, 1.000000000000000000, 0.9510565162951535312, 1.000000000000000000, 0.9510565162951535312, 1.000000000000000000, 0.9510565162951535312, 1.000000000000000000, 0.9510565162951535312, 1.000000000000000000, 0.9510565162951535312, 1.000000000000000000, 0.9510565162951535312, 1.000000000000000000, 0.9510565162951535312, 1.000000000000000000, 0.9510565162951535312, 1.000000000000000000, 0.9510565162951535312, 1.000000000000000000, 0.9510565162951535312, 1.000000000000000000, 0.9510565162951535312, 1.000000000000000000, 0.9510565162951535312, 1.000000000000000000, 0.9510565162951535312, 1.000000000000000000, 0.9510565162951535312, 1.000000000000000000, 0.9510565162951535312, 1.000000000000000000, 0.9510565162951535312, 1.000000000000000000, 0.9510565162951535312, 1.000000000000000000, 0.9510565162951535312, 1.000000000000000000, 0.9510565162951535312, 1.000000000000000000, 0.9510565162951535312, 1.000000000000000000, 0.9510565162951535312, 1.000000000000000000, 0.9510565162951535312, 1.000000000000000000, 0.9510565162951535312, 1.000000000000000000, 0.9510565162951535312, 1.000000000000000000, 0.9510565162951535312, 1.000000000000000000, 0.9510565162951535312, 1.000000000000000000, 0.9510565162951535312, 1.000000000000000000, 0.9510565162951535312, 1.000000000000000000, 0.9510565162951535312, 1.000000000000000000, 0.9510565162951535312, 1.000000000000000000, 0.9510565162951535312, 1.000000000000000000, 0.9510565162951535312, 1.000000000000000000, 0.9510565162951535312, 1.000000000000000000, 0.9510565162951535312, 1.000000000000000000, 0.9510565162951535312, 1.000000000000000000, 0.9510565162951535312, 1.000000000000000000, 0.9510565162951535312, 1.000000000000000000, 0.9510565162951535312, 1.000000000000000000, 0.9510565162951535312, 1.000000000000000000, 0.9510565162951535312, 1.000000000000000000, 0.9510565162951535312, 1.000000000000000000, 0.9510565162951535312, 1.000000000000000000, 0.9510565162951535312, 1.000000000000000000, 0.9510565162951535312, 1.000000000000000000, 0.9510565162951535312, 1.000000000000000000, 0.9510565162951535312, 1.000000000000000000, 0.9510565162951535312, 1.000000000000000000, 0.9510565162951535312, 1.000000000000000000, 0.9510565162951535312, 1.000000000000000000, 0.9510565162951535312, 1.000000000000000000, 0.9510565162951535312, 1.000000000000000000, 0.9510565162951535312, 1.000000000000000000, 0.9510565162951535312, 1.000000000000000000, 0.9510565162951535312, 1.000000000000000000, 0.9510565162951535312, 1.000000000000000000, 0.9510565162951535312, 1.000000000000000000, 0.9510565162951535312, 1.000000000000000000, 0.9510565162951535312, 1.000000000000000000, 0.9510565162951535312, 1.000000000000000000, 0.9510565162951535312, 1.000000000000000000, 0.9510565162951535312, 1.000000000000000000, 0.9510565162951535312, 1.000000000000000000, 0.9510565162951535312, 1.000000000000000000, 0.9510565162951535312, 1.000000000000000000, 0.9510565162951535312, 1.000000000000000000, 0.9510565162951535312, 1.000000000000000000, 0.9510565162951535312, 1.000000000000000000, 0.9510565162951535312, 1.000000000000000000, 0.9510565162951535312, 1.000000000000000000) ) ) 
 REPRESENTATION_ITEM ( '' )  SURFACE ( )  );
#4289 = CARTESIAN_POINT ( 'NONE',  ( 30.90169943749474157, 41.30000000000001137, -42.53254041760200721 ) ) ;
#4290 = CARTESIAN_POINT ( 'NONE',  ( -30.90169943749473802, 24.08125000068279675, 42.53254041760200721 ) ) ;
#4291 = CARTESIAN_POINT ( 'NONE',  ( 40.34137639590981905, 42.72187500034139873, 29.30972558990010768 ) ) ;
#4292 = EDGE_CURVE ( 'NONE', #6085, #10405, #7038, .T. ) ;
#4293 = CARTESIAN_POINT ( 'NONE',  ( 30.81806926056964002, 26.62187500034139731, 42.41743335407647209 ) ) ;
#4294 = CARTESIAN_POINT ( 'NONE',  ( 2.500000000000000000, 244.0000000000000284, -49.99999999999999289 ) ) ;
#4295 = ORIENTED_EDGE ( 'NONE', *, *, #657, .T. ) ;
#4296 = CARTESIAN_POINT ( 'NONE',  ( -3.219174618344376363E-15, 31.28125000068279604, -52.57311121191334990 ) ) ;
#4297 = EDGE_CURVE ( 'NONE', #6400, #12892, #11556, .T. ) ;
#4298 = EDGE_LOOP ( 'NONE', ( #16151, #2919, #2565, #11055, #3341 ) ) ;
#4299 = LINE ( 'NONE', #14341, #15282 ) ;
#4300 = DIRECTION ( 'NONE',  ( 5.069245582283711292E-17, 1.000000000000000000, -8.780190904559502465E-17 ) ) ;
#4301 = ADVANCED_FACE ( 'NONE', ( #4221 ), #9288, .T. ) ;
#4302 = CARTESIAN_POINT ( 'NONE',  ( -7.919222016226934890, 34.22999571913595673, 49.99999999999996447 ) ) ;
#4303 = CARTESIAN_POINT ( 'NONE',  ( 49.86468353125000164, 46.92187500034139447, -6.106662507704105588E-15 ) ) ;
#4304 = CARTESIAN_POINT ( 'NONE',  ( 49.86468353125000164, 24.85937500034139802, -6.106662507704105588E-15 ) ) ;
#4305 = CARTESIAN_POINT ( 'NONE',  ( -1.240322475938754499E-13, 36.28125000068280315, 50.00000000000000000 ) ) ;
#4306 = CARTESIAN_POINT ( 'NONE',  ( -30.81806926056963292, 41.62187500034139020, -42.41743335407646498 ) ) ;
#4307 = CARTESIAN_POINT ( 'NONE',  ( -9.023094029599238268E-16, 65.00000000000001421, 6.590543865931048246E-16 ) ) ;
#4308 = CARTESIAN_POINT ( 'NONE',  ( 9.631387414534489405E-15, 46.42187500034139447, 52.43083105670540789 ) ) ;
#4309 = CARTESIAN_POINT ( 'NONE',  ( -40.45084971874737079, 45.98125000068279888, 29.38926261462367151 ) ) ;
#4310 = EDGE_LOOP ( 'NONE', ( #14073, #7050, #15037, #14295 ) ) ;
#4311 = CARTESIAN_POINT ( 'NONE',  ( 49.86468353124999453, 41.02187500034139589, -16.20201782572376459 ) ) ;
#4312 = VERTEX_POINT ( 'NONE', #2960 ) ;
#4313 = ORIENTED_EDGE ( 'NONE', *, *, #1100, .T. ) ;
#4314 = EDGE_CURVE ( 'NONE', #7369, #13993, #13783, .T. ) ;
#4315 = DIRECTION ( 'NONE',  ( 0.000000000000000000, 0.000000000000000000, -1.000000000000000000 ) ) ;
#4316 = CARTESIAN_POINT ( 'NONE',  ( 50.00000000000000711, 38.68125000068280173, 16.24598481164530739 ) ) ;
#4317 = EDGE_CURVE ( 'NONE', #13593, #2563, #14910, .T. ) ;
#4318 = PLANE ( 'NONE',  #14478 ) ;
#4319 = CARTESIAN_POINT ( 'NONE',  ( 15.45084971874736723, 27.40000000000000213, -47.55282581475768211 ) ) ;
#4320 = CARTESIAN_POINT ( 'NONE',  ( -49.86468353124999453, 41.95937500034138878, 16.20201782572377525 ) ) ;
#4321 = CARTESIAN_POINT ( 'NONE',  ( -7.919222016226804328, 26.22999571913594963, 50.00000000000000000 ) ) ;
#4322 = CARTESIAN_POINT ( 'NONE',  ( 0.5000000000000000000, 245.0000000000000284, 49.99999999999999289 ) ) ;
#4323 = FACE_OUTER_BOUND ( 'NONE', #5068, .T. ) ;
#4324 = DIRECTION ( 'NONE',  ( 0.000000000000000000, -1.000000000000000000, 0.000000000000000000 ) ) ;
#4325 = CARTESIAN_POINT ( 'NONE',  ( -30.90169943749474868, 35.48125000068279888, -42.53254041760200721 ) ) ;
#4326 = DIRECTION ( 'NONE',  ( -1.000000000000000000, 0.000000000000000000, 0.000000000000000000 ) ) ;
#4327 = VECTOR ( 'NONE', #13055, 999.9999999999998863 ) ;
#4328 = CARTESIAN_POINT ( 'NONE',  ( 5.026048470455315886, 27.47395152954465658, -39.76282541253125657 ) ) ;
#4329 = CARTESIAN_POINT ( 'NONE',  ( 43.87482193696061472, 257.0000000000001137, 10.00000000000000178 ) ) ;
#4330 = ORIENTED_EDGE ( 'NONE', *, *, #6165, .T. ) ;
#4331 = CARTESIAN_POINT ( 'NONE',  ( -49.86468353124999453, 37.75937500034140015, -16.20201782572375393 ) ) ;
#4332 = VERTEX_POINT ( 'NONE', #4626 ) ;
#4333 = ORIENTED_EDGE ( 'NONE', *, *, #3107, .T. ) ;
#4334 = EDGE_CURVE ( 'NONE', #10001, #12012, #3708, .T. ) ;
#4335 = CARTESIAN_POINT ( 'NONE',  ( -30.90169943749474868, 49.48125000068279178, -42.53254041760200721 ) ) ;
#4336 = EDGE_CURVE ( 'NONE', #1001, #11210, #12057, .T. ) ;
#4337 = DIRECTION ( 'NONE',  ( 0.000000000000000000, 0.000000000000000000, -1.000000000000000000 ) ) ;
#4338 = CARTESIAN_POINT ( 'NONE',  ( 49.86468353125001585, 22.75937500034139660, 16.20201782572375038 ) ) ;
#4340 = VERTEX_POINT ( 'NONE', #8687 ) ;
#4339 = AXIS2_PLACEMENT_3D ( 'NONE', #12987, #1591, #6685 ) ;
#4341 = CARTESIAN_POINT ( 'NONE',  ( 19.99999999999999645, 312.0000000000000568, 2.500000000000002220 ) ) ;
#4342 = CARTESIAN_POINT ( 'NONE',  ( 49.99999999999999289, 23.10000000000000142, -16.24598481164532160 ) ) ;
#4343 = CARTESIAN_POINT ( 'NONE',  ( 5.000000000000000000, 120.2608755106154348, -31.08930263536150562 ) ) ;
#4344 = CARTESIAN_POINT ( 'NONE',  ( 49.86468353125001585, 30.82187500034139660, 16.20201782572375038 ) ) ;
#4345 = EDGE_CURVE ( 'NONE', #6737, #12652, #6014, .T. ) ;
#4346 = CARTESIAN_POINT ( 'NONE',  ( -50.00000000000000000, 37.78125000068280315, 0.000000000000000000 ) ) ;
#4347 = FACE_OUTER_BOUND ( 'NONE', #4834, .T. ) ;
#4348 = DIRECTION ( 'NONE',  ( -0.000000000000000000, -1.000000000000000000, -0.000000000000000000 ) ) ;
#4349 = CARTESIAN_POINT ( 'NONE',  ( 49.86468353125000164, 20.92187500034139802, -6.106662507704105588E-15 ) ) ;
#4350 = CARTESIAN_POINT ( 'NONE',  ( 2.939893647802748866, 6.264020653511243708, 102.0000000000000142 ) ) ;
#4351 = CARTESIAN_POINT ( 'NONE',  ( 50.00000000000000000, 33.00000000000000000, -6.123233995736766085E-15 ) ) ;
#4352 = CARTESIAN_POINT ( 'NONE',  ( -15.40903463028481646, 31.45937500034139944, -47.42413220539093999 ) ) ;
#4353 = AXIS2_PLACEMENT_3D ( 'NONE', #16293, #4929, #9984 ) ;
#4354 = CARTESIAN_POINT ( 'NONE',  ( 1.293669679204937499E-13, 39.50000000000000711, -50.00000000000000000 ) ) ;
#4355 = EDGE_LOOP ( 'NONE', ( #15233, #14760, #6174 ) ) ;
#4356 = CARTESIAN_POINT ( 'NONE',  ( 40.34137639590981905, 28.65937500034139873, 29.30972558990010768 ) ) ;
#4357 = ORIENTED_EDGE ( 'NONE', *, *, #626, .T. ) ;
#4358 = CARTESIAN_POINT ( 'NONE',  ( -47.28673853953970507, 260.3313524089090265, 10.00000000000000178 ) ) ;
#4359 = CARTESIAN_POINT ( 'NONE',  ( 30.81806926056964002, 40.55937500034139731, 42.41743335407647209 ) ) ;
#4360 = CARTESIAN_POINT ( 'NONE',  ( 25.50583519765999796, 284.7842439685853719, 3.511670395308114312 ) ) ;
#4361 = VECTOR ( 'NONE', #1152, 1000.000000000000000 ) ;
#4362 = CARTESIAN_POINT ( 'NONE',  ( -24.78235906513968345, 286.0218276481963358, 7.282359065138694909 ) ) ;
#4363 = CARTESIAN_POINT ( 'NONE',  ( -3.210462471511496205E-15, 35.42187500034140157, -52.43083105670540789 ) ) ;
#4364 = CARTESIAN_POINT ( 'NONE',  ( -40.34137639590981195, 36.05937500034139731, 29.30972558990012189 ) ) ;
#4365 = CARTESIAN_POINT ( 'NONE',  ( -30.90169943749473447, 44.30000000000000426, 42.53254041760200721 ) ) ;
#4366 = CARTESIAN_POINT ( 'NONE',  ( -15.40903463028481646, 29.52187500034139589, -47.42413220539093999 ) ) ;
#4367 = CARTESIAN_POINT ( 'NONE',  ( 50.00000000000000711, 40.89999999999999858, 16.24598481164530739 ) ) ;
#4368 = CARTESIAN_POINT ( 'NONE',  ( 9.657523855033129090E-15, 24.28125000068279959, 52.57311121191334990 ) ) ;
#4369 = CARTESIAN_POINT ( 'NONE',  ( 15.40903463028482356, 46.52187500034139589, 47.42413220539093999 ) ) ;
#4370 = CARTESIAN_POINT ( 'NONE',  ( 30.81806926056964002, 24.62187500034139731, 42.41743335407647209 ) ) ;
#4371 = CIRCLE ( 'NONE', #3574, 100.0000000000000000 ) ;
#4372 = CARTESIAN_POINT ( 'NONE',  ( -30.81806926056962226, 48.15937500034139873, 42.41743335407647209 ) ) ;
#4373 = ORIENTED_EDGE ( 'NONE', *, *, #16278, .F. ) ;
#4374 = CARTESIAN_POINT ( 'NONE',  ( 50.00000000000000711, 32.68125000068279462, 16.24598481164530739 ) ) ;
#4375 = VERTEX_POINT ( 'NONE', #8518 ) ;
#4376 = CARTESIAN_POINT ( 'NONE',  ( -7.919222016226818539, 49.33250428222964956, -49.99999999999999289 ) ) ;
#4377 =( BOUNDED_CURVE ( )  B_SPLINE_CURVE ( 2, ( #1150, #11313, #5580, #152, #5341, #9139, #12880, #4161, #1729, #7809, #11879, #9386, #9231 ),
 .UNSPECIFIED., .F., .T. ) 
 B_SPLINE_CURVE_WITH_KNOTS ( ( 3, 2, 2, 2, 2, 2, 3 ),
 ( 0.5833333333333333703, 0.5866666666666666696, 0.5933333333333333792, 0.5999999999999999778, 0.6066666666666666874, 0.6133333333333332860, 0.6166666666666666963 ),
 .UNSPECIFIED. ) 
 CURVE ( )  GEOMETRIC_REPRESENTATION_ITEM ( )  RATIONAL_B_SPLINE_CURVE ( ( 0.9755282581475768211, 0.9755282581475771542, 1.000000000000000000, 0.9510565162951535312, 1.000000000000000000, 0.9510565162951535312, 1.000000000000000000, 0.9510565162951535312, 1.000000000000000000, 0.9510565162951535312, 1.000000000000000000, 0.9755282581475763770, 0.9755282581475768211 ) ) 
 REPRESENTATION_ITEM ( '' )  );
#4378 = EDGE_CURVE ( 'NONE', #16375, #9704, #4416, .T. ) ;
#4379 = CARTESIAN_POINT ( 'NONE',  ( -8.880528407616480990, 25.91118970470954963, 102.0000000000000142 ) ) ;
#4380 = CARTESIAN_POINT ( 'NONE',  ( 9.631387414534489405E-15, 40.42187500034138736, 52.43083105670540789 ) ) ;
#4381 = CARTESIAN_POINT ( 'NONE',  ( -49.86468353124999453, 23.95937500034138878, 16.20201782572377525 ) ) ;
#4382 = PLANE ( 'NONE',  #385 ) ;
#4383 = VECTOR ( 'NONE', #4923, 1000.000000000000000 ) ;
#4384 = ITEM_DEFINED_TRANSFORMATION ( 'NONE', 'NONE', #11317,  #15812 ) ;
#4385 = CARTESIAN_POINT ( 'NONE',  ( 40.45084971874737789, 38.80000000000000426, 29.38926261462365375 ) ) ;
#4386 = ADVANCED_FACE ( 'NONE', ( #13423 ), #15923, .T. ) ;
#4387 = EDGE_CURVE ( 'NONE', #12652, #6737, #13752, .T. ) ;
#4388 = CARTESIAN_POINT ( 'NONE',  ( 30.81806926056962936, 49.22187500034139873, -42.41743335407647209 ) ) ;
#4389 = ORIENTED_EDGE ( 'NONE', *, *, #4643, .T. ) ;
#4390 = CARTESIAN_POINT ( 'NONE',  ( -40.34137639590981195, 44.12187500034139731, 29.30972558990012189 ) ) ;
#4391 = ADVANCED_FACE ( 'NONE', ( #2366 ), #9608, .F. ) ;
#4392 = ORIENTED_EDGE ( 'NONE', *, *, #8165, .T. ) ;
#4393 = ORIENTED_EDGE ( 'NONE', *, *, #2274, .F. ) ;
#4394 = CIRCLE ( 'NONE', #13670, 17.50000000000000000 ) ;
#4395 = DIRECTION ( 'NONE',  ( 0.000000000000000000, 1.000000000000000000, 0.000000000000000000 ) ) ;
#4396 = CYLINDRICAL_SURFACE ( 'NONE', #10509, 50.00000000000000000 ) ;
#4397 = CARTESIAN_POINT ( 'NONE',  ( 5.510910596163089556E-15, 247.0000000000000284, -45.00000000000000000 ) ) ;
#4398 = CARTESIAN_POINT ( 'NONE',  ( 40.45084971874737079, 21.19999999999999929, -29.38926261462366440 ) ) ;
#4399 = CARTESIAN_POINT ( 'NONE',  ( -15.40903463028481646, 43.45937500034139589, -47.42413220539093999 ) ) ;
#4400 = CARTESIAN_POINT ( 'NONE',  ( -3.210462471511496205E-15, 47.35937500034138736, -52.43083105670540789 ) ) ;
#4401 = FACE_OUTER_BOUND ( 'NONE', #16328, .T. ) ;
#4402 = FACE_OUTER_BOUND ( 'NONE', #3434, .T. ) ;
#4403 = PRESENTATION_STYLE_ASSIGNMENT (( #2984 ) ) ;
#4404 = CARTESIAN_POINT ( 'NONE',  ( 8.880528407616436581, 25.91118970470966687, 101.0000000000000000 ) ) ;
#4405 = LINE ( 'NONE', #7226, #3649 ) ;
#4406 = AXIS2_PLACEMENT_3D ( 'NONE', #5389, #4300, #2791 ) ;
#4407 = DIRECTION ( 'NONE',  ( -0.8660254037844363761, -0.5000000000000039968, 0.000000000000000000 ) ) ;
#4408 = DIRECTION ( 'NONE',  ( -0.3090169943749448977, -0.9510565162951543083, 0.000000000000000000 ) ) ;
#4409 = ORIENTED_EDGE ( 'NONE', *, *, #3632, .T. ) ;
#4410 = CARTESIAN_POINT ( 'NONE',  ( 40.34137639590981195, 29.05937500034139376, -29.30972558990011834 ) ) ;
#4411 = EDGE_LOOP ( 'NONE', ( #13539, #5003 ) ) ;
#4412 = ORIENTED_EDGE ( 'NONE', *, *, #13630, .F. ) ;
#4413 = ORIENTED_EDGE ( 'NONE', *, *, #73, .T. ) ;
#4414 = CARTESIAN_POINT ( 'NONE',  ( 30.90169943749473802, 43.30000000000000426, -42.53254041760200721 ) ) ;
#4415 = CIRCLE ( 'NONE', #2817, 45.00000000000000000 ) ;
#4416 = CIRCLE ( 'NONE', #7060, 79.49773270518484480 ) ;
#4417 = AXIS2_PLACEMENT_3D ( 'NONE', #82, #6, #1509 ) ;
#4418 = CARTESIAN_POINT ( 'NONE',  ( 7.499999999999998224, 25.00000000000000355, 24.29058411375428150 ) ) ;
#4419 = CARTESIAN_POINT ( 'NONE',  ( 15.40903463028481113, 21.25937500034139660, -47.42413220539094709 ) ) ;
#4420 = VECTOR ( 'NONE', #5683, 1000.000000000000114 ) ;
#4421 = VECTOR ( 'NONE', #7485, 999.9999999999998863 ) ;
#4422 = VERTEX_POINT ( 'NONE', #14740 ) ;
#4423 = PRODUCT_DEFINITION_SHAPE ( 'NONE', 'NONE',  #16468 ) ;
#4424 = CARTESIAN_POINT ( 'NONE',  ( -50.00000000000000000, 49.78125000068280315, 0.000000000000000000 ) ) ;
#4425 = CARTESIAN_POINT ( 'NONE',  ( 2.600676159226420495E-13, 23.50000000000000000, -49.99999999999999289 ) ) ;
#4426 = PRESENTATION_LAYER_ASSIGNMENT (  '', '', ( #13426 ) ) ;
#4427 = CARTESIAN_POINT ( 'NONE',  ( 9.881733417930924190, 8.048309972292271297, 102.0000000000000142 ) ) ;
#4428 = CARTESIAN_POINT ( 'NONE',  ( -15.40903463028480580, 30.32187500034140015, 47.42413220539094709 ) ) ;
#4429 = DIRECTION ( 'NONE',  ( 1.000000000000000000, 7.930164461608261426E-16, 0.000000000000000000 ) ) ;
#4430 = CARTESIAN_POINT ( 'NONE',  ( 13.22646626819541282, 11.02685957165896014, 97.16024423813598787 ) ) ;
#4431 = CARTESIAN_POINT ( 'NONE',  ( 0.000000000000000000, 272.0000000000000000, 0.000000000000000000 ) ) ;
#4432 = CARTESIAN_POINT ( 'NONE',  ( -15.40903463028480580, 24.32187500034139660, 47.42413220539094709 ) ) ;
#4433 = DIRECTION ( 'NONE',  ( -0.2079116908177665313, 0.9781476007338041345, 0.000000000000000000 ) ) ;
#4434 = CARTESIAN_POINT ( 'NONE',  ( -30.90169943749474868, 33.69999999999998863, -42.53254041760200721 ) ) ;
#4435 = CARTESIAN_POINT ( 'NONE',  ( 40.34137639590981195, 27.05937500034139731, -29.30972558990011834 ) ) ;
#4436 = AXIS2_PLACEMENT_3D ( 'NONE', #9671, #7184, #848 ) ;
#4437 = AXIS2_PLACEMENT_3D ( 'NONE', #2308, #9629, #15018 ) ;
#4438 = VECTOR ( 'NONE', #14211, 1000.000000000000000 ) ;
#4439 = CARTESIAN_POINT ( 'NONE',  ( -40.45084971874737789, 29.80000000000000071, -29.38926261462365730 ) ) ;
#4440 = EDGE_LOOP ( 'NONE', ( #13781, #2936, #8530, #15266 ) ) ;
#4441 = UNCERTAINTY_MEASURE_WITH_UNIT (LENGTH_MEASURE( 1.000000000000000082E-05 ), #7325, 'distance_accuracy_value', 'NONE');
#4442 = CARTESIAN_POINT ( 'NONE',  ( -30.81806926056963292, 31.55937500034139376, -42.41743335407646498 ) ) ;
#4443 = ADVANCED_FACE ( 'NONE', ( #8440 ), #7198, .T. ) ;
#4444 = ORIENTED_EDGE ( 'NONE', *, *, #5655, .F. ) ;
#4445 = CYLINDRICAL_SURFACE ( 'NONE', #14482, 50.00000000000000000 ) ;
#4446 = CARTESIAN_POINT ( 'NONE',  ( 15.40903463028481113, 39.25937500034140015, -47.42413220539094709 ) ) ;
#4447 = CIRCLE ( 'NONE', #13718, 10.00000000000000000 ) ;
#4448 = VECTOR ( 'NONE', #1191, 1000.000000000000000 ) ;
#4449 = CARTESIAN_POINT ( 'NONE',  ( -40.34137639590981195, 20.12187500034139731, 29.30972558990012189 ) ) ;
#4450 = AXIS2_PLACEMENT_3D ( 'NONE', #4821, #14594, #10874 ) ;
#4451 = CARTESIAN_POINT ( 'NONE',  ( -25.66084200511936686, 284.4942466288902096, 3.821684010227676342 ) ) ;
#4452 = CARTESIAN_POINT ( 'NONE',  ( -49.86468353125000164, 27.92187500034139447, 0.000000000000000000 ) ) ;
#4453 = CARTESIAN_POINT ( 'NONE',  ( -30.81806926056962226, 36.15937500034139163, 42.41743335407647209 ) ) ;
#4454 = CARTESIAN_POINT ( 'NONE',  ( -15.45084971874736368, 44.39999999999999858, 47.55282581475768211 ) ) ;
#4455 = CARTESIAN_POINT ( 'NONE',  ( 40.34137639590981905, 28.72187500034139873, 29.30972558990010768 ) ) ;
#4456 = CARTESIAN_POINT ( 'NONE',  ( 49.99999999999999289, 43.10000000000000142, -16.24598481164532160 ) ) ;
#4457 = CARTESIAN_POINT ( 'NONE',  ( -40.34137639590981905, 45.65937500034139873, -29.30972558990011478 ) ) ;
#4458 = CARTESIAN_POINT ( 'NONE',  ( -49.86468353124999453, 45.82187500034140015, -16.20201782572375393 ) ) ;
#4459 = CARTESIAN_POINT ( 'NONE',  ( 30.90169943749475578, 48.69999999999999574, 42.53254041760200010 ) ) ;
#4460 = EDGE_LOOP ( 'NONE', ( #1584, #16260, #2, #8764 ) ) ;
#4461 = CARTESIAN_POINT ( 'NONE',  ( -40.34137639590981905, 49.65937500034139873, -29.30972558990011478 ) ) ;
#4462 = EDGE_LOOP ( 'NONE', ( #2789, #14991, #12051, #16393, #13020, #2688 ) ) ;
#4463 = ORIENTED_EDGE ( 'NONE', *, *, #7428, .F. ) ;
#4464 = CARTESIAN_POINT ( 'NONE',  ( 9.657523855033129090E-15, 32.28125000068279604, 52.57311121191334990 ) ) ;
#4465 = ORIENTED_EDGE ( 'NONE', *, *, #7682, .T. ) ;
#4466 = LINE ( 'NONE', #9443, #4960 ) ;
#4467 = CARTESIAN_POINT ( 'NONE',  ( 15.45084971874737789, 32.38125000068280457, 47.55282581475767500 ) ) ;
#4468 = CARTESIAN_POINT ( 'NONE',  ( -49.86468353124999453, 37.82187500034139305, -16.20201782572375393 ) ) ;
#4469 = CARTESIAN_POINT ( 'NONE',  ( -49.86468353125000164, 47.92187500034139447, 0.000000000000000000 ) ) ;
#4470 = CARTESIAN_POINT ( 'NONE',  ( 0.000000000000000000, 22.50000000000000000, 102.0000000000000142 ) ) ;
#4471 = ADVANCED_FACE ( 'NONE', ( #5301 ), #16343, .T. ) ;
#4472 = CONTEXT_DEPENDENT_SHAPE_REPRESENTATION ( #4103, #4423 ) ;
#4473 = CARTESIAN_POINT ( 'NONE',  ( -30.90169943749473802, 36.29999999999998295, 42.53254041760200721 ) ) ;
#4474 = CARTESIAN_POINT ( 'NONE',  ( 9.631387414534489405E-15, 40.42187500034138736, 52.43083105670540789 ) ) ;
#4475 = CARTESIAN_POINT ( 'NONE',  ( -15.45084971874736368, 46.18125000068280173, 47.55282581475768211 ) ) ;
#4476 = VERTEX_POINT ( 'NONE', #10274 ) ;
#4477 = CARTESIAN_POINT ( 'NONE',  ( -40.34137639590981195, 40.12187500034139731, 29.30972558990012189 ) ) ;
#4478 = ORIENTED_EDGE ( 'NONE', *, *, #6749, .F. ) ;
#4479 = ORIENTED_EDGE ( 'NONE', *, *, #399, .T. ) ;
#4480 =( BOUNDED_CURVE ( )  B_SPLINE_CURVE ( 2, ( #8218, #7057, #16022, #11043, #10714, #883, #5977, #4650, #9715, #16113, #4745, #14853, #13284, #12032, #3481, #14679, #3398, #13606, #15942, #2132, #5729, #2211, #11957, #555, #9471, #4400, #14521, #8374, #634, #13448, #10805, #4488, #8464, #9553, #2057, #3223, #4564, #14600, #12122, #727, #9627, #7145, #806, #2695, #1363, #1050, #3561, #8707, #6534, #6625, #970, #2778, #7851, #11600, #197, #12931, #1536, #11678, #8614, #13687, #276, #5380, #10435, #11513, #16197, #15491, #4116, #9185, #14249, #7308, #4825, #12367, #6066, #15332, #11135, #9025, #9880, #14931, #10352, #2304, #10276, #13772, #12843, #11216, #7392, #14080, #6144, #12456, #9102, #7694, #1446, #16271, #4902, #9960, #15016, #3651, #2619, #5303, #7771, #15414, #12764, #4032, #6454, #5216, #109, #3951, #14162, #3023, #13250, #14565, #7936, #6872, #13169, #4286, #8094, #9518, #5691, #1778, #13087, #1612, #596, #6790, #11923, #523, #2946, #6705, #5618, #5456, #10681, #15733, #1928, #11834, #11755, #14329, #3189, #356, #1693, #4453, #4364, #5546, #9429, #14477, #3112, #8184, #445, #1850, #10521, #15583, #10608, #12075, #8013, #12000, #7021, #8262, #10759, #4208, #6946, #15819, #13326, #679, #5778, #9274, #15664, #9350, #10844, #4532, #15908, #14400, #9595, #13009, #2868, #9926, #16159, #768, #3609, #1014, #8669, #929, #5942, #8506, #2351, #3270, #4790, #13490, #8340, #16236, #14813, #3525, #10922, #9673, #7433, #12500, #850, #13738, #8577, #14898, #2260, #8428, #1093, #9846, #13402, #6185, #13571, #3444, #11259, #2098, #16317, #4952, #4610, #2014, #14642, #9766, #15984, #7356, #7271, #12247, #14980, #7186, #7111, #11005, #2175, #6027, #16067, #4700, #12327, #13652, #11099, #12423, #6111, #11182, #4870, #5858, #12166, #14723, #3354, #8752, #10248, #15310, #6353, #7673, #10169, #9003, #3932, #7831, #13815, #11339, #2597, #1263, #5114, #15219, #14061, #11419, #11491, #3849, #179, #11572, #12, #1341, #2756, #16406, #7504, #2427, #5039, #2677, #12575, #5193, #8914, #3770, #6268, #13979, #7751, #9084, #3696, #5283, #10334, #12820, #1421, #15394, #4014, #14140, #10094, #12906, #1173, #1516, #6606, #12744, #15142, #11660, #257, #6432, #89, #6514, #10011, #15067, #8829, #13892, #2508, #7587, #12665, #11816, #13148 ),
 .UNSPECIFIED., .F., .F. ) 
 B_SPLINE_CURVE_WITH_KNOTS ( ( 3, 2, 2, 2, 2, 2, 2, 2, 2, 2, 2, 2, 2, 2, 2, 2, 2, 2, 2, 2, 2, 2, 2, 2, 2, 2, 2, 2, 2, 2, 2, 2, 2, 2, 2, 2, 2, 2, 2, 2, 2, 2, 2, 2, 2, 2, 2, 2, 2, 2, 2, 2, 2, 2, 2, 2, 2, 2, 2, 2, 2, 2, 2, 2, 2, 2, 2, 2, 2, 2, 2, 2, 2, 2, 2, 2, 2, 2, 2, 2, 2, 2, 2, 2, 2, 2, 2, 2, 2, 2, 2, 2, 2, 2, 2, 2, 2, 2, 2, 2, 2, 2, 2, 2, 2, 2, 2, 2, 2, 2, 2, 2, 2, 2, 2, 2, 2, 2, 2, 2, 2, 2, 2, 2, 2, 2, 2, 2, 2, 2, 2, 2, 2, 2, 2, 2, 2, 2, 2, 2, 2, 2, 2, 2, 2, 2, 2, 2, 2, 2, 3 ),
 ( 0.000000000000000000, 0.006666666666666667095, 0.01333333333333333419, 0.02000000000000000042, 0.02666666666666666838, 0.03333333333333333287, 0.04000000000000000083, 0.04666666666666666879, 0.05333333333333333676, 0.05999999999999999778, 0.06666666666666666574, 0.07333333333333333370, 0.08000000000000000167, 0.08666666666666666963, 0.09333333333333333759, 0.1000000000000000056, 0.1066666666666666735, 0.1133333333333333276, 0.1199999999999999956, 0.1266666666666666774, 0.1333333333333333315, 0.1400000000000000133, 0.1466666666666666674, 0.1533333333333333215, 0.1600000000000000033, 0.1666666666666666574, 0.1733333333333333393, 0.1799999999999999933, 0.1866666666666666752, 0.1933333333333333293, 0.2000000000000000111, 0.2066666666666666652, 0.2133333333333333470, 0.2200000000000000011, 0.2266666666666666552, 0.2333333333333333370, 0.2399999999999999911, 0.2466666666666666730, 0.2533333333333333548, 0.2600000000000000089, 0.2666666666666666630, 0.2733333333333333171, 0.2800000000000000266, 0.2866666666666666807, 0.2933333333333333348, 0.2999999999999999889, 0.3066666666666666430, 0.3133333333333333526, 0.3200000000000000067, 0.3266666666666666607, 0.3333333333333333148, 0.3400000000000000244, 0.3466666666666666785, 0.3533333333333333326, 0.3599999999999999867, 0.3666666666666666408, 0.3733333333333333504, 0.3800000000000000044, 0.3866666666666666585, 0.3933333333333333126, 0.4000000000000000222, 0.4066666666666666763, 0.4133333333333333304, 0.4199999999999999845, 0.4266666666666666941, 0.4333333333333333481, 0.4400000000000000022, 0.4466666666666666563, 0.4533333333333333104, 0.4600000000000000200, 0.4666666666666666741, 0.4733333333333333282, 0.4799999999999999822, 0.4866666666666666918, 0.4933333333333333459, 0.5000000000000000000, 0.5066666666666667096, 0.5133333333333333082, 0.5200000000000000178, 0.5266666666666666163, 0.5333333333333333259, 0.5400000000000000355, 0.5466666666666666341, 0.5533333333333333437, 0.5600000000000000533, 0.5666666666666666519, 0.5733333333333333615, 0.5799999999999999600, 0.5866666666666666696, 0.5933333333333333792, 0.5999999999999999778, 0.6066666666666666874, 0.6133333333333332860, 0.6199999999999999956, 0.6266666666666667052, 0.6333333333333333037, 0.6400000000000000133, 0.6466666666666666119, 0.6533333333333333215, 0.6600000000000000311, 0.6666666666666666297, 0.6733333333333333393, 0.6800000000000000488, 0.6866666666666666474, 0.6933333333333333570, 0.6999999999999999556, 0.7066666666666666652, 0.7133333333333333748, 0.7199999999999999734, 0.7266666666666666829, 0.7333333333333332815, 0.7399999999999999911, 0.7466666666666667007, 0.7533333333333332993, 0.7600000000000000089, 0.7666666666666667185, 0.7733333333333333171, 0.7800000000000000266, 0.7866666666666666252, 0.7933333333333333348, 0.8000000000000000444, 0.8066666666666666430, 0.8133333333333333526, 0.8199999999999999512, 0.8266666666666666607, 0.8333333333333333703, 0.8399999999999999689, 0.8466666666666666785, 0.8533333333333333881, 0.8599999999999999867, 0.8666666666666666963, 0.8733333333333332948, 0.8800000000000000044, 0.8866666666666667140, 0.8933333333333333126, 0.9000000000000000222, 0.9066666666666666208, 0.9133333333333333304, 0.9200000000000000400, 0.9266666666666666385, 0.9333333333333333481, 0.9399999999999999467, 0.9466666666666666563, 0.9533333333333333659, 0.9599999999999999645, 0.9666666666666666741, 0.9733333333333333837, 0.9799999999999999822, 0.9866666666666666918, 0.9933333333333332904, 0.9953403926135619972 ),
 .UNSPECIFIED. ) 
 CURVE ( )  GEOMETRIC_REPRESENTATION_ITEM ( )  RATIONAL_B_SPLINE_CURVE ( ( 1.000000000000000000, 0.9510565162951535312, 1.000000000000000000, 0.9510565162951535312, 1.000000000000000000, 0.9510565162951535312, 1.000000000000000000, 0.9510565162951535312, 1.000000000000000000, 0.9510565162951535312, 1.000000000000000000, 0.9510565162951535312, 1.000000000000000000, 0.9510565162951535312, 1.000000000000000000, 0.9510565162951535312, 1.000000000000000000, 0.9510565162951535312, 1.000000000000000000, 0.9510565162951535312, 1.000000000000000000, 0.9510565162951535312, 1.000000000000000000, 0.9510565162951535312, 1.000000000000000000, 0.9510565162951535312, 1.000000000000000000, 0.9510565162951535312, 1.000000000000000000, 0.9510565162951535312, 1.000000000000000000, 0.9510565162951535312, 1.000000000000000000, 0.9510565162951535312, 1.000000000000000000, 0.9510565162951535312, 1.000000000000000000, 0.9510565162951535312, 1.000000000000000000, 0.9510565162951535312, 1.000000000000000000, 0.9510565162951535312, 1.000000000000000000, 0.9510565162951535312, 1.000000000000000000, 0.9510565162951535312, 1.000000000000000000, 0.9510565162951535312, 1.000000000000000000, 0.9510565162951535312, 1.000000000000000000, 0.9510565162951535312, 1.000000000000000000, 0.9510565162951535312, 1.000000000000000000, 0.9510565162951535312, 1.000000000000000000, 0.9510565162951535312, 1.000000000000000000, 0.9510565162951535312, 1.000000000000000000, 0.9510565162951535312, 1.000000000000000000, 0.9510565162951535312, 1.000000000000000000, 0.9510565162951535312, 1.000000000000000000, 0.9510565162951535312, 1.000000000000000000, 0.9510565162951535312, 1.000000000000000000, 0.9510565162951535312, 1.000000000000000000, 0.9510565162951535312, 1.000000000000000000, 0.9510565162951535312, 1.000000000000000000, 0.9510565162951535312, 1.000000000000000000, 0.9510565162951535312, 1.000000000000000000, 0.9510565162951535312, 1.000000000000000000, 0.9510565162951535312, 1.000000000000000000, 0.9510565162951535312, 1.000000000000000000, 0.9510565162951535312, 1.000000000000000000, 0.9510565162951535312, 1.000000000000000000, 0.9510565162951535312, 1.000000000000000000, 0.9510565162951535312, 1.000000000000000000, 0.9510565162951535312, 1.000000000000000000, 0.9510565162951535312, 1.000000000000000000, 0.9510565162951535312, 1.000000000000000000, 0.9510565162951535312, 1.000000000000000000, 0.9510565162951535312, 1.000000000000000000, 0.9510565162951535312, 1.000000000000000000, 0.9510565162951535312, 1.000000000000000000, 0.9510565162951535312, 1.000000000000000000, 0.9510565162951535312, 1.000000000000000000, 0.9510565162951535312, 1.000000000000000000, 0.9510565162951535312, 1.000000000000000000, 0.9510565162951535312, 1.000000000000000000, 0.9510565162951535312, 1.000000000000000000, 0.9510565162951535312, 1.000000000000000000, 0.9510565162951535312, 1.000000000000000000, 0.9510565162951535312, 1.000000000000000000, 0.9510565162951535312, 1.000000000000000000, 0.9510565162951535312, 1.000000000000000000, 0.9510565162951535312, 1.000000000000000000, 0.9510565162951535312, 1.000000000000000000, 0.9510565162951535312, 1.000000000000000000, 0.9510565162951535312, 1.000000000000000000, 0.9510565162951535312, 1.000000000000000000, 0.9510565162951535312, 1.000000000000000000, 0.9510565162951535312, 1.000000000000000000, 0.9510565162951535312, 1.000000000000000000, 0.9510565162951535312, 1.000000000000000000, 0.9510565162951535312, 1.000000000000000000, 0.9510565162951535312, 1.000000000000000000, 0.9510565162951535312, 1.000000000000000000, 0.9510565162951535312, 1.000000000000000000, 0.9510565162951535312, 1.000000000000000000, 0.9510565162951535312, 1.000000000000000000, 0.9510565162951535312, 1.000000000000000000, 0.9510565162951535312, 1.000000000000000000, 0.9510565162951535312, 1.000000000000000000, 0.9510565162951535312, 1.000000000000000000, 0.9510565162951535312, 1.000000000000000000, 0.9510565162951535312, 1.000000000000000000, 0.9510565162951535312, 1.000000000000000000, 0.9510565162951535312, 1.000000000000000000, 0.9510565162951535312, 1.000000000000000000, 0.9510565162951535312, 1.000000000000000000, 0.9510565162951535312, 1.000000000000000000, 0.9510565162951535312, 1.000000000000000000, 0.9510565162951535312, 1.000000000000000000, 0.9510565162951535312, 1.000000000000000000, 0.9510565162951535312, 1.000000000000000000, 0.9510565162951535312, 1.000000000000000000, 0.9510565162951535312, 1.000000000000000000, 0.9510565162951535312, 1.000000000000000000, 0.9510565162951535312, 1.000000000000000000, 0.9510565162951535312, 1.000000000000000000, 0.9510565162951535312, 1.000000000000000000, 0.9510565162951535312, 1.000000000000000000, 0.9510565162951535312, 1.000000000000000000, 0.9510565162951535312, 1.000000000000000000, 0.9510565162951535312, 1.000000000000000000, 0.9510565162951535312, 1.000000000000000000, 0.9510565162951535312, 1.000000000000000000, 0.9510565162951535312, 1.000000000000000000, 0.9510565162951535312, 1.000000000000000000, 0.9510565162951535312, 1.000000000000000000, 0.9510565162951535312, 1.000000000000000000, 0.9510565162951535312, 1.000000000000000000, 0.9510565162951535312, 1.000000000000000000, 0.9510565162951535312, 1.000000000000000000, 0.9510565162951535312, 1.000000000000000000, 0.9510565162951535312, 1.000000000000000000, 0.9510565162951535312, 1.000000000000000000, 0.9510565162951535312, 1.000000000000000000, 0.9510565162951535312, 1.000000000000000000, 0.9510565162951535312, 1.000000000000000000, 0.9510565162951535312, 1.000000000000000000, 0.9510565162951535312, 1.000000000000000000, 0.9510565162951535312, 1.000000000000000000, 0.9510565162951535312, 1.000000000000000000, 0.9510565162951535312, 1.000000000000000000, 0.9510565162951535312, 1.000000000000000000, 0.9510565162951535312, 1.000000000000000000, 0.9510565162951535312, 1.000000000000000000, 0.9510565162951535312, 1.000000000000000000, 0.9510565162951535312, 1.000000000000000000, 0.9510565162951535312, 1.000000000000000000, 0.9510565162951535312, 1.000000000000000000, 0.9510565162951535312, 1.000000000000000000, 0.9510565162951535312, 1.000000000000000000, 0.9510565162951535312, 1.000000000000000000, 0.9510565162951535312, 1.000000000000000000, 0.9510565162951535312, 1.000000000000000000, 0.9510565162951535312, 1.000000000000000000, 0.9510565162951535312, 1.000000000000000000, 0.9510565162951535312, 1.000000000000000000, 0.9510565162951535312, 1.000000000000000000, 0.9510565162951535312, 1.000000000000000000, 0.9510565162951535312, 1.000000000000000000, 0.9510565162951535312, 1.000000000000000000, 0.9510565162951535312, 1.000000000000000000, 0.9510565162951535312, 1.000000000000000000, 0.9510565162951535312, 1.000000000000000000, 0.9510565162951535312, 1.000000000000000000, 0.9510565162951535312, 1.000000000000000000, 0.9852651290235199255, 0.9794023859079349359 ) ) 
 REPRESENTATION_ITEM ( '' )  );
#4481 = ORIENTED_EDGE ( 'NONE', *, *, #15955, .F. ) ;
#4482 = ADVANCED_FACE ( 'NONE', ( #10189 ), #9023, .T. ) ;
#4483 = DIRECTION ( 'NONE',  ( 0.000000000000000000, 0.000000000000000000, -1.000000000000000000 ) ) ;
#4484 = CARTESIAN_POINT ( 'NONE',  ( 15.40544456622774661, 14.18301270189236973, 101.0000000000000000 ) ) ;
#4485 = LINE ( 'NONE', #16349, #13418 ) ;
#4486 = DIRECTION ( 'NONE',  ( 0.000000000000000000, 0.000000000000000000, 1.000000000000000000 ) ) ;
#4487 = CARTESIAN_POINT ( 'NONE',  ( 40.34137639590981905, 42.65937500034139873, 29.30972558990010768 ) ) ;
#4488 = CARTESIAN_POINT ( 'NONE',  ( 49.86468353125001585, 46.75937500034140015, 16.20201782572375038 ) ) ;
#4489 = CARTESIAN_POINT ( 'NONE',  ( -40.45084971874737079, 33.98125000068279888, 29.38926261462367151 ) ) ;
#4490 = AXIS2_PLACEMENT_3D ( 'NONE', #12722, #11547, #3992 ) ;
#4491 = EDGE_CURVE ( 'NONE', #12980, #7494, #8769, .T. ) ;
#4492 = LINE ( 'NONE', #2215, #11519 ) ;
#4493 = CARTESIAN_POINT ( 'NONE',  ( -15.45084971874736368, 36.18125000068280173, 47.55282581475768211 ) ) ;
#4494 = CARTESIAN_POINT ( 'NONE',  ( 7.919222016226854954, 42.33250428222964246, 49.99999999999998579 ) ) ;
#4495 = DIRECTION ( 'NONE',  ( 0.000000000000000000, 0.000000000000000000, 1.000000000000000000 ) ) ;
#4496 = ORIENTED_EDGE ( 'NONE', *, *, #16426, .F. ) ;
#4497 = ADVANCED_FACE ( 'NONE', ( #12841 ), #1281, .T. ) ;
#4498 = CARTESIAN_POINT ( 'NONE',  ( -15.40903463028481646, 33.45937500034139589, -47.42413220539093999 ) ) ;
#4499 = VERTEX_POINT ( 'NONE', #6371 ) ;
#4500 = ORIENTED_EDGE ( 'NONE', *, *, #10739, .F. ) ;
#4501 = ORIENTED_EDGE ( 'NONE', *, *, #6710, .F. ) ;
#4502 = CARTESIAN_POINT ( 'NONE',  ( -49.99999999999999289, 43.88125000068279746, 16.24598481164533226 ) ) ;
#4503 = AXIS2_PLACEMENT_3D ( 'NONE', #13711, #10901, #7411 ) ;
#4504 = CARTESIAN_POINT ( 'NONE',  ( -40.45084971874737789, 39.80000000000000426, -29.38926261462365730 ) ) ;
#4505 = CARTESIAN_POINT ( 'NONE',  ( 0.000000000000000000, 52.26146722824297797, 0.000000000000000000 ) ) ;
#4506 = ORIENTED_EDGE ( 'NONE', *, *, #7834, .T. ) ;
#4507 = DIRECTION ( 'NONE',  ( 1.000000000000000000, 0.000000000000000000, 0.000000000000000000 ) ) ;
#4508 = FACE_OUTER_BOUND ( 'NONE', #5232, .T. ) ;
#4509 = DIRECTION ( 'NONE',  ( 2.312964634635742464E-16, 0.000000000000000000, -1.000000000000000000 ) ) ;
#4510 = DIRECTION ( 'NONE',  ( 0.000000000000000000, 0.000000000000000000, 1.000000000000000000 ) ) ;
#4511 = DIRECTION ( 'NONE',  ( 0.000000000000000000, 1.000000000000000000, 0.000000000000000000 ) ) ;
#4512 = CARTESIAN_POINT ( 'NONE',  ( -40.45084971874737079, 48.20000000000000284, 29.38926261462367151 ) ) ;
#4513 = ADVANCED_FACE ( 'NONE', ( #1106 ), #13999, .T. ) ;
#4514 = PLANE ( 'NONE',  #6474 ) ;
#4515 = DIRECTION ( 'NONE',  ( 0.000000000000000000, 0.000000000000000000, -1.000000000000000000 ) ) ;
#4516 = CARTESIAN_POINT ( 'NONE',  ( 40.34137639590981195, 25.12187500034139376, -29.30972558990011834 ) ) ;
#4517 = CARTESIAN_POINT ( 'NONE',  ( 7.571758127758665857, 38.27715053026751946, 101.0000000000000000 ) ) ;
#4518 = AXIS2_PLACEMENT_3D ( 'NONE', #1965, #5812, #4565 ) ;
#4519 = CARTESIAN_POINT ( 'NONE',  ( -40.45084971874737789, 33.80000000000000426, -29.38926261462365730 ) ) ;
#4520 = CARTESIAN_POINT ( 'NONE',  ( -3.210462471511496205E-15, 23.35937500034139802, -52.43083105670540789 ) ) ;
#4521 = B_SPLINE_CURVE_WITH_KNOTS ( 'NONE', 3,
 ( #8639, #989, #2236, #2325 ),
 .UNSPECIFIED., .F., .F.,
 ( 4, 4 ),
 ( 2.829004760679149478E-07, 0.001414802801989367221 ),
 .UNSPECIFIED. ) ;
#4522 = CARTESIAN_POINT ( 'NONE',  ( -49.86468353125000164, 49.85937500034139447, 0.000000000000000000 ) ) ;
#4523 = ORIENTED_EDGE ( 'NONE', *, *, #16244, .F. ) ;
#4524 = CARTESIAN_POINT ( 'NONE',  ( 45.11452830843730766, 25.00000000000000355, -21.24066852005663719 ) ) ;
#4525 = ORIENTED_EDGE ( 'NONE', *, *, #205, .F. ) ;
#4526 = FACE_OUTER_BOUND ( 'NONE', #2749, .T. ) ;
#4527 = CARTESIAN_POINT ( 'NONE',  ( 40.34137639590981905, 38.65937500034139873, 29.30972558990010768 ) ) ;
#4528 = EDGE_CURVE ( 'NONE', #894, #15230, #9100, .T. ) ;
#4529 = CARTESIAN_POINT ( 'NONE',  ( 24.99999979512263693, 287.0011899277170073, 7.499999795122639590 ) ) ;
#4530 = CYLINDRICAL_SURFACE ( 'NONE', #7074, 2.000000000000001776 ) ;
#4531 = CARTESIAN_POINT ( 'NONE',  ( 49.86468353125001585, 28.82187500034139305, 16.20201782572375038 ) ) ;
#4532 = CARTESIAN_POINT ( 'NONE',  ( -3.210462471511496205E-15, 33.35937500034139447, -52.43083105670540789 ) ) ;
#4533 = CARTESIAN_POINT ( 'NONE',  ( -40.45084971874737079, 36.20000000000000284, 29.38926261462367151 ) ) ;
#4534 = CARTESIAN_POINT ( 'NONE',  ( -40.34137639590981195, 32.12187500034140442, 29.30972558990012189 ) ) ;
#4535 = PLANE ( 'NONE',  #14750 ) ;
#4536 = CARTESIAN_POINT ( 'NONE',  ( 40.34137639590981195, 43.05937500034139731, -29.30972558990011834 ) ) ;
#4537 = CARTESIAN_POINT ( 'NONE',  ( -15.40903463028481646, 45.52187500034139589, -47.42413220539093999 ) ) ;
#4538 = CARTESIAN_POINT ( 'NONE',  ( 30.81806926056964002, 22.62187500034139731, 42.41743335407647209 ) ) ;
#4539 = ORIENTED_EDGE ( 'NONE', *, *, #2349, .F. ) ;
#4540 = CARTESIAN_POINT ( 'NONE',  ( -40.34137639590981195, 48.05937500034139731, 29.30972558990012189 ) ) ;
#4541 = ORIENTED_EDGE ( 'NONE', *, *, #14844, .T. ) ;
#4542 = ORIENTED_EDGE ( 'NONE', *, *, #2775, .F. ) ;
#4543 = CARTESIAN_POINT ( 'NONE',  ( -40.45084971874737079, 33.98125000068279888, 29.38926261462367151 ) ) ;
#4544 = ORIENTED_EDGE ( 'NONE', *, *, #14807, .T. ) ;
#4545 = DIRECTION ( 'NONE',  ( 0.9781476007338070211, -0.2079116908177531808, -0.000000000000000000 ) ) ;
#4546 = CARTESIAN_POINT ( 'NONE',  ( 30.81806926056964002, 40.62187500034139731, 42.41743335407646498 ) ) ;
#4547 = CARTESIAN_POINT ( 'NONE',  ( -49.86468353124999453, 45.82187500034140015, -16.20201782572375393 ) ) ;
#4548 = FACE_OUTER_BOUND ( 'NONE', #1563, .T. ) ;
#4549 = CARTESIAN_POINT ( 'NONE',  ( -40.34137639590981195, 22.12187500034139731, 29.30972558990012189 ) ) ;
#4550 = ITEM_DEFINED_TRANSFORMATION ( 'NONE', 'NONE', #10261,  #15812 ) ;
#4551 = CARTESIAN_POINT ( 'NONE',  ( 40.45084971874737789, 36.79999999999999716, 29.38926261462365375 ) ) ;
#4552 = CARTESIAN_POINT ( 'NONE',  ( -15.40903463028481646, 41.52187500034139589, -47.42413220539093999 ) ) ;
#4553 = CARTESIAN_POINT ( 'NONE',  ( -7.919222016226822092, 46.22999571913594963, 50.00000000000000000 ) ) ;
#4554 = ORIENTED_EDGE ( 'NONE', *, *, #794, .F. ) ;
#4555 = CARTESIAN_POINT ( 'NONE',  ( 15.40903463028481113, 39.32187500034140015, -47.42413220539094709 ) ) ;
#4556 = EDGE_LOOP ( 'NONE', ( #15723, #8270, #13295 ) ) ;
#4557 = ORIENTED_EDGE ( 'NONE', *, *, #4278, .T. ) ;
#4558 = ORIENTED_EDGE ( 'NONE', *, *, #12595, .T. ) ;
#4559 = FACE_OUTER_BOUND ( 'NONE', #12107, .T. ) ;
#4560 = CARTESIAN_POINT ( 'NONE',  ( 5.000000000000000000, 90.81335289333328831, 3.860273862222790342 ) ) ;
#4561 = DIRECTION ( 'NONE',  ( 0.000000000000000000, -1.000000000000000000, 0.000000000000000000 ) ) ;
#4562 = CARTESIAN_POINT ( 'NONE',  ( -15.45084971874736368, 20.40000000000000213, 47.55282581475768211 ) ) ;
#4563 = CARTESIAN_POINT ( 'NONE',  ( -15.40903463028480580, 36.25937500034140015, 47.42413220539094709 ) ) ;
#4564 = CARTESIAN_POINT ( 'NONE',  ( -15.40903463028480580, 46.25937500034140015, 47.42413220539094709 ) ) ;
#4565 = DIRECTION ( 'NONE',  ( 0.000000000000000000, 0.000000000000000000, -1.000000000000000000 ) ) ;
#4566 = CARTESIAN_POINT ( 'NONE',  ( -2.499999999999999556, 242.0000000000000284, 49.17157287525379417 ) ) ;
#4567 = CARTESIAN_POINT ( 'NONE',  ( 0.000000000000000000, 22.50000000000000000, 101.0000000000000000 ) ) ;
#4568 = CARTESIAN_POINT ( 'NONE',  ( -24.78626291527393377, 25.00000000000000355, -5.650101528493794767 ) ) ;
#4569 = CARTESIAN_POINT ( 'NONE',  ( 50.00000000000000000, 37.00000000000000711, -6.123233995736766085E-15 ) ) ;
#4570 = CARTESIAN_POINT ( 'NONE',  ( 7.919222016226758143, 36.55125428154683931, 50.00000000000000711 ) ) ;
#4571 = ORIENTED_EDGE ( 'NONE', *, *, #11373, .F. ) ;
#4572 =( BOUNDED_CURVE ( )  B_SPLINE_CURVE ( 2, ( #6106, #1088, #8745, #3520, #11254 ),
 .UNSPECIFIED., .F., .F. ) 
 B_SPLINE_CURVE_WITH_KNOTS ( ( 3, 2, 3 ),
 ( 0.9833333333333333925, 0.9866666666666666918, 0.9926850605967240115 ),
 .UNSPECIFIED. ) 
 CURVE ( )  GEOMETRIC_REPRESENTATION_ITEM ( )  RATIONAL_B_SPLINE_CURVE ( ( 0.9755282581475768211, 0.9755282581475771542, 1.000000000000000000, 0.9558158252132334942, 0.9914069812288479611 ) ) 
 REPRESENTATION_ITEM ( '' )  );
#4573 = CARTESIAN_POINT ( 'NONE',  ( -40.34137639590981195, 28.05937500034139731, 29.30972558990012189 ) ) ;
#4574 = ORIENTED_EDGE ( 'NONE', *, *, #13150, .T. ) ;
#4575 = ORIENTED_EDGE ( 'NONE', *, *, #5307, .T. ) ;
#4576 = ORIENTED_EDGE ( 'NONE', *, *, #204, .T. ) ;
#4577 = CARTESIAN_POINT ( 'NONE',  ( 40.45084971874737789, 42.58125000068280031, 29.38926261462365375 ) ) ;
#4578 = CARTESIAN_POINT ( 'NONE',  ( -49.86468353125000164, 49.92187500034140157, 0.000000000000000000 ) ) ;
#4579 = PLANE ( 'NONE',  #9956 ) ;
#4580 = VERTEX_POINT ( 'NONE', #12685 ) ;
#4581 = CARTESIAN_POINT ( 'NONE',  ( -1.240322475938754499E-13, 38.50000000000000711, 50.00000000000000000 ) ) ;
#4582 = CARTESIAN_POINT ( 'NONE',  ( -16.61395733222127191, 16.88676649784340711, 95.59049725886258386 ) ) ;
#4583 = FACE_OUTER_BOUND ( 'NONE', #6617, .T. ) ;
#4584 = CARTESIAN_POINT ( 'NONE',  ( 49.72257916183961868, 96.64601816452534422, 5.000000000000000000 ) ) ;
#4585 = DIRECTION ( 'NONE',  ( 0.000000000000000000, 0.000000000000000000, 1.000000000000000000 ) ) ;
#4586 = EDGE_CURVE ( 'NONE', #10689, #13617, #5409, .T. ) ;
#4587 = DIRECTION ( 'NONE',  ( 0.000000000000000000, 0.000000000000000000, -1.000000000000000000 ) ) ;
#4588 = CARTESIAN_POINT ( 'NONE',  ( 2.978552182361884590E-14, 47.50000000000000711, -50.00000000000000000 ) ) ;
#4589 = CARTESIAN_POINT ( 'NONE',  ( -45.11452830843730766, 20.00000000000000711, 21.24066852005664430 ) ) ;
#4590 = CARTESIAN_POINT ( 'NONE',  ( 15.40903463028481113, 21.32187500034139660, -47.42413220539094709 ) ) ;
#4591 = PLANE ( 'NONE',  #10558 ) ;
#4592 = ADVANCED_FACE ( 'NONE', ( #3949 ), #2616, .F. ) ;
#4593 = CARTESIAN_POINT ( 'NONE',  ( 50.00000000000000000, 27.00000000000000355, -6.123233995736766085E-15 ) ) ;
#4594 = CARTESIAN_POINT ( 'NONE',  ( -49.86468353125000164, 27.85937500034139447, 0.000000000000000000 ) ) ;
#4595 = EDGE_CURVE ( 'NONE', #11668, #9978, #14160, .T. ) ;
#4596 = ADVANCED_FACE ( 'NONE', ( #16423 ), #8377, .T. ) ;
#4597 = CARTESIAN_POINT ( 'NONE',  ( -2.500000000000000000, 217.0000000000000284, -44.93050188902856945 ) ) ;
#4598 = ORIENTED_EDGE ( 'NONE', *, *, #7340, .F. ) ;
#4599 = CONICAL_SURFACE ( 'NONE', #11745, 89.49773270518483059, 0.1745329251994333364 ) ;
#4600 = ADVANCED_FACE ( 'NONE', ( #4972 ), #8937, .T. ) ;
#4601 = UNCERTAINTY_MEASURE_WITH_UNIT (LENGTH_MEASURE( 1.000000000000000082E-05 ), #8405, 'distance_accuracy_value', 'NONE');
#4602 = CARTESIAN_POINT ( 'NONE',  ( 16.45433951800531247, 21.27333336794017171, 102.0000000000000142 ) ) ;
#4603 = EDGE_LOOP ( 'NONE', ( #4478, #4523, #5751, #8023, #2627, #12773, #14732, #11520, #9320, #3180, #4145, #2991, #13336, #12627, #11801, #9300, #3643, #2722, #13559, #9952, #2923, #3261, #3279, #8587, #13037, #3213, #14447, #2004, #1508, #12090, #6138, #6401, #12588, #7366 ) ) ;
#4604 = CARTESIAN_POINT ( 'NONE',  ( 0.000000000000000000, 25.00000000000000355, 0.000000000000000000 ) ) ;
#4605 = CARTESIAN_POINT ( 'NONE',  ( -15.40903463028481646, 33.45937500034139589, -47.42413220539093999 ) ) ;
#4606 = DIRECTION ( 'NONE',  ( 0.000000000000000000, 1.000000000000000000, 0.000000000000000000 ) ) ;
#4607 = CARTESIAN_POINT ( 'NONE',  ( -1.240322475938754499E-13, 40.50000000000000000, 50.00000000000000000 ) ) ;
#4608 = CARTESIAN_POINT ( 'NONE',  ( 1.293669679204937499E-13, 39.50000000000000711, -50.00000000000000000 ) ) ;
#4609 = CARTESIAN_POINT ( 'NONE',  ( -40.34137639590981905, 31.72187500034139873, -29.30972558990011478 ) ) ;
#4610 = CARTESIAN_POINT ( 'NONE',  ( 40.34137639590981195, 29.05937500034139376, -29.30972558990011834 ) ) ;
#4611 = DIRECTION ( 'NONE',  ( 0.000000000000000000, 1.000000000000000000, 0.000000000000000000 ) ) ;
#4612 = CARTESIAN_POINT ( 'NONE',  ( 49.86468353125001585, 28.82187500034139305, 16.20201782572375038 ) ) ;
#4613 = FACE_OUTER_BOUND ( 'NONE', #6526, .T. ) ;
#4614 = CIRCLE ( 'NONE', #6994, 2.000000000000001776 ) ;
#4615 = CARTESIAN_POINT ( 'NONE',  ( 15.40903463028481113, 47.25937500034140015, -47.42413220539094709 ) ) ;
#4616 = CARTESIAN_POINT ( 'NONE',  ( 49.86468353124999453, 35.02187500034139589, -16.20201782572376459 ) ) ;
#4617 = CARTESIAN_POINT ( 'NONE',  ( 30.81806926056964002, 20.62187500034139020, 42.41743335407647209 ) ) ;
#4618 = ADVANCED_FACE ( 'NONE', ( #10031, #12594 ), #15330, .F. ) ;
#4619 = EDGE_LOOP ( 'NONE', ( #8127, #405, #4257, #288 ) ) ;
#4620 = CARTESIAN_POINT ( 'NONE',  ( -15.40903463028481646, 45.45937500034139589, -47.42413220539093999 ) ) ;
#4621 = EDGE_LOOP ( 'NONE', ( #840, #11868, #5108, #8104, #5406 ) ) ;
#4622 = EDGE_CURVE ( 'NONE', #11153, #5800, #12168, .T. ) ;
#4623 = CARTESIAN_POINT ( 'NONE',  ( -15.45084971874737256, 27.38125000068280102, -47.55282581475767500 ) ) ;
#4624 = CIRCLE ( 'NONE', #10973, 16.50000000000000711 ) ;
#4625 = ORIENTED_EDGE ( 'NONE', *, *, #9567, .T. ) ;
#4626 = CARTESIAN_POINT ( 'NONE',  ( 10.68655108903834794, 8.641875097208380652, 101.0000000000000000 ) ) ;
#4627 = CARTESIAN_POINT ( 'NONE',  ( 49.86468353125001585, 42.82187500034139305, 16.20201782572375038 ) ) ;
#4628 = CARTESIAN_POINT ( 'NONE',  ( -15.40903463028480580, 20.25937500034139660, 47.42413220539094709 ) ) ;
#4629 = PLANE ( 'NONE',  #9706 ) ;
#4630 = CARTESIAN_POINT ( 'NONE',  ( 40.34137639590981905, 22.72187500034139518, 29.30972558990010768 ) ) ;
#4631 = CONTEXT_DEPENDENT_SHAPE_REPRESENTATION ( #15766, #13036 ) ;
#4632 = CARTESIAN_POINT ( 'NONE',  ( 15.45084971874737789, 34.38125000068280457, 47.55282581475767500 ) ) ;
#4633 = CARTESIAN_POINT ( 'NONE',  ( 15.45084971874737789, 38.60000000000000142, 47.55282581475767500 ) ) ;
#4634 = CARTESIAN_POINT ( 'NONE',  ( -15.40903463028480580, 40.32187500034140015, 47.42413220539094709 ) ) ;
#4635 = PLANE ( 'NONE',  #2189 ) ;
#4636 = ORIENTED_EDGE ( 'NONE', *, *, #7662, .F. ) ;
#4637 = CARTESIAN_POINT ( 'NONE',  ( 30.81806926056964002, 42.62187500034139731, 42.41743335407647209 ) ) ;
#4638 = CARTESIAN_POINT ( 'NONE',  ( -49.99999999999999289, 41.68125000068280173, -16.24598481164531449 ) ) ;
#4639 = ORIENTED_EDGE ( 'NONE', *, *, #5117, .F. ) ;
#4640 = ORIENTED_EDGE ( 'NONE', *, *, #14631, .T. ) ;
#4641 = EDGE_CURVE ( 'NONE', #798, #15902, #30, .T. ) ;
#4642 = ORIENTED_EDGE ( 'NONE', *, *, #9388, .F. ) ;
#4643 = EDGE_CURVE ( 'NONE', #9526, #4080, #16099, .T. ) ;
#4644 = LINE ( 'NONE', #5889, #15591 ) ;
#4645 = CARTESIAN_POINT ( 'NONE',  ( 16.48218589020105185, 28.38111794481774908, 101.0000000000000000 ) ) ;
#4646 = VECTOR ( 'NONE', #1530, 1000.000000000000000 ) ;
#4647 = CARTESIAN_POINT ( 'NONE',  ( 15.45084971874737789, 26.60000000000000142, 47.55282581475767500 ) ) ;
#4648 = CARTESIAN_POINT ( 'NONE',  ( -49.99999999999999289, 20.09999999999999787, 16.24598481164533226 ) ) ;
#4649 = CARTESIAN_POINT ( 'NONE',  ( 40.34137639590981905, 34.65937500034139873, 29.30972558990010768 ) ) ;
#4650 = CARTESIAN_POINT ( 'NONE',  ( 30.81806926056962936, 49.15937500034139163, -42.41743335407646498 ) ) ;
#4651 = DIRECTION ( 'NONE',  ( -0.000000000000000000, -1.000000000000000000, -0.000000000000000000 ) ) ;
#4652 = CARTESIAN_POINT ( 'NONE',  ( 2.600676159226421000E-13, 33.28125000068279604, -49.99999999999999289 ) ) ;
#4653 = CARTESIAN_POINT ( 'NONE',  ( -5.823736356558309156E-14, 44.50000000000000000, 50.00000000000000000 ) ) ;
#4654 = CARTESIAN_POINT ( 'NONE',  ( 5.288637809679021457E-15, 52.00000000000001421, -35.00000000000002842 ) ) ;
#4655 = CARTESIAN_POINT ( 'NONE',  ( -2.547328955960238000E-13, 34.50000000000000000, 49.99999999999999289 ) ) ;
#4656 = CARTESIAN_POINT ( 'NONE',  ( 17.34476375915451740, 20.17423772944865945, 101.0000000000000000 ) ) ;
#4657 = ORIENTED_EDGE ( 'NONE', *, *, #14015, .T. ) ;
#4658 = CIRCLE ( 'NONE', #13660, 35.00000000000000711 ) ;
#4659 = CARTESIAN_POINT ( 'NONE',  ( 40.34137639590981195, 31.05937500034139731, -29.30972558990011834 ) ) ;
#4660 = EDGE_LOOP ( 'NONE', ( #12509, #4277, #12222, #12384 ) ) ;
#4661 = ORIENTED_EDGE ( 'NONE', *, *, #13801, .T. ) ;
#4662 = ORIENTED_EDGE ( 'NONE', *, *, #8269, .F. ) ;
#4663 = CARTESIAN_POINT ( 'NONE',  ( -40.45084971874737789, 43.58125000068280031, -29.38926261462365730 ) ) ;
#4664 = DIRECTION ( 'NONE',  ( 0.000000000000000000, 1.000000000000000000, 0.000000000000000000 ) ) ;
#4665 = CARTESIAN_POINT ( 'NONE',  ( 40.45084971874737789, 28.80000000000000426, 29.38926261462365375 ) ) ;
#4666 = ORIENTED_EDGE ( 'NONE', *, *, #294, .F. ) ;
#4667 = CARTESIAN_POINT ( 'NONE',  ( -30.90169943749473447, 48.08125000068279320, 42.53254041760200721 ) ) ;
#4668 = CARTESIAN_POINT ( 'NONE',  ( 8.446640517145639571E-15, 28.28125000068279959, 50.00000000000000000 ) ) ;
#4669 = CARTESIAN_POINT ( 'NONE',  ( -10.75298028539202200, 8.646267545471964411, 97.89130469945834534 ) ) ;
#4670 = CYLINDRICAL_SURFACE ( 'NONE', #12393, 50.00000000000000000 ) ;
#4671 = DIRECTION ( 'NONE',  ( -0.000000000000000000, -1.000000000000000000, -0.000000000000000000 ) ) ;
#4672 = DIRECTION ( 'NONE',  ( 0.000000000000000000, 1.000000000000000000, 0.000000000000000000 ) ) ;
#4673 = VECTOR ( 'NONE', #5576, 1000.000000000000000 ) ;
#4674 = DIRECTION ( 'NONE',  ( 1.000000000000000000, 0.000000000000000000, 0.000000000000000000 ) ) ;
#4675 = CARTESIAN_POINT ( 'NONE',  ( 49.99999999999999289, 36.88125000068279036, -16.24598481164532160 ) ) ;
#4676 =( GEOMETRIC_REPRESENTATION_CONTEXT ( 3 ) GLOBAL_UNCERTAINTY_ASSIGNED_CONTEXT ( ( #10912 ) ) GLOBAL_UNIT_ASSIGNED_CONTEXT ( ( #1575, #5503, #9475 ) ) REPRESENTATION_CONTEXT ( 'NONE', 'WORKASPACE' ) );
#4677 = CARTESIAN_POINT ( 'NONE',  ( -45.60931600130317776, 20.00000000000001066, 20.15700215907655135 ) ) ;
#4678 = CARTESIAN_POINT ( 'NONE',  ( -40.34137639590981905, 23.72187500034139873, -29.30972558990011478 ) ) ;
#4679 =( BOUNDED_CURVE ( )  B_SPLINE_CURVE ( 3, ( #1199, #117, #15251, #8864 ),
 .UNSPECIFIED., .F., .F. ) 
 B_SPLINE_CURVE_WITH_KNOTS ( ( 4, 4 ),
 ( 2.558501865821646959, 3.141592653589793116 ),
 .UNSPECIFIED. ) 
 CURVE ( )  GEOMETRIC_REPRESENTATION_ITEM ( )  RATIONAL_B_SPLINE_CURVE ( ( 1.000000000000000000, 0.9718672150731668680, 0.9718672150731668680, 1.000000000000000000 ) ) 
 REPRESENTATION_ITEM ( '' )  );
#4680 = PLANE ( 'NONE',  #6048 ) ;
#4681 = B_SPLINE_CURVE_WITH_KNOTS ( 'NONE', 3,
 ( #2063, #3152, #5586, #7065 ),
 .UNSPECIFIED., .F., .F.,
 ( 4, 4 ),
 ( 2.829004760709176796E-07, 0.001414802801989367871 ),
 .UNSPECIFIED. ) ;
#4682 = CARTESIAN_POINT ( 'NONE',  ( 15.45084971874737789, 30.60000000000000142, 47.55282581475767500 ) ) ;
#4683 = CARTESIAN_POINT ( 'NONE',  ( -15.40903463028480580, 26.25937500034140015, 47.42413220539094709 ) ) ;
#4684 = CARTESIAN_POINT ( 'NONE',  ( -7.919222016226773242, 42.22999571913594963, 50.00000000000000711 ) ) ;
#4685 = DIRECTION ( 'NONE',  ( 0.000000000000000000, 0.000000000000000000, -1.000000000000000000 ) ) ;
#4686 = ORIENTED_EDGE ( 'NONE', *, *, #4087, .F. ) ;
#4687 = CONICAL_SURFACE ( 'NONE', #150, 16.50000000000000711, 0.7853981633974447263 ) ;
#4688 = VECTOR ( 'NONE', #11977, 1000.000000000000114 ) ;
#4689 = CARTESIAN_POINT ( 'NONE',  ( -30.81806926056963292, 25.55937500034139376, -42.41743335407646498 ) ) ;
#4690 = ORIENTED_EDGE ( 'NONE', *, *, #8627, .F. ) ;
#4691 = LINE ( 'NONE', #15133, #16373 ) ;
#4692 = CARTESIAN_POINT ( 'NONE',  ( 40.34137639590981905, 36.65937500034139873, 29.30972558990010768 ) ) ;
#4693 = CARTESIAN_POINT ( 'NONE',  ( 50.00000000000000000, 40.78125000068279604, -6.123233995736766085E-15 ) ) ;
#4694 = EDGE_CURVE ( 'NONE', #14169, #2087, #13757, .T. ) ;
#4695 = CARTESIAN_POINT ( 'NONE',  ( 15.45084971874736723, 35.39999999999999858, -47.55282581475768211 ) ) ;
#4696 = ADVANCED_FACE ( 'NONE', ( #6622 ), #10679, .F. ) ;
#4697 = DIRECTION ( 'NONE',  ( 0.000000000000000000, 0.000000000000000000, 1.000000000000000000 ) ) ;
#4698 = CLOSED_SHELL ( 'NONE', ( #6928, #10284, #4060, #14884, #6739, #4301, #3878, #8847, #2661, #10035, #10518, #14607, #11167, #11202, #1019, #613, #6021, #12253, #3471, #13850, #5707, #11911, #1323, #84, #15145, #9635, #11125, #4837, #12291, #9610, #10662, #9826, #11496 ) ) ;
#4699 = CARTESIAN_POINT ( 'NONE',  ( -3.210462471511496205E-15, 31.42187500034139447, -52.43083105670540789 ) ) ;
#4700 = CARTESIAN_POINT ( 'NONE',  ( -30.81806926056963292, 27.55937500034139376, -42.41743335407646498 ) ) ;
#4701 = AXIS2_PLACEMENT_3D ( 'NONE', #7750, #8667, #10168 ) ;
#4702 = AXIS2_PLACEMENT_3D ( 'NONE', #8053, #1966, #13365 ) ;
#4703 = DIRECTION ( 'NONE',  ( 0.000000000000000000, 0.000000000000000000, -1.000000000000000000 ) ) ;
#4704 = CARTESIAN_POINT ( 'NONE',  ( -15.40903463028480580, 28.32187500034139660, 47.42413220539094709 ) ) ;
#4705 = AXIS2_PLACEMENT_3D ( 'NONE', #15903, #10676, #15575 ) ;
#4706 = CARTESIAN_POINT ( 'NONE',  ( 50.00000000000000711, 32.89999999999999858, 16.24598481164530739 ) ) ;
#4707 = ADVANCED_FACE ( 'NONE', ( #2866 ), #10503, .T. ) ;
#4708 = CARTESIAN_POINT ( 'NONE',  ( 40.34137639590981195, 45.05937500034139731, -29.30972558990011834 ) ) ;
#4709 = CARTESIAN_POINT ( 'NONE',  ( -49.86468353124999453, 37.82187500034139305, -16.20201782572375393 ) ) ;
#4710 = ORIENTED_EDGE ( 'NONE', *, *, #12618, .F. ) ;
#4711 = CARTESIAN_POINT ( 'NONE',  ( 15.40903463028481113, 21.32187500034139660, -47.42413220539094709 ) ) ;
#4712 = VERTEX_POINT ( 'NONE', #11003 ) ;
#4713 = EDGE_CURVE ( 'NONE', #9419, #3904, #15566, .T. ) ;
#4714 = CARTESIAN_POINT ( 'NONE',  ( -40.34137639590981905, 43.65937500034139163, -29.30972558990011478 ) ) ;
#4715 = AXIS2_PLACEMENT_3D ( 'NONE', #13895, #6517, #10172 ) ;
#4716 = VERTEX_POINT ( 'NONE', #3441 ) ;
#4717 = CIRCLE ( 'NONE', #16368, 17.50000000000000000 ) ;
#4718 = AXIS2_PLACEMENT_3D ( 'NONE', #6244, #14179, #6164 ) ;
#4720 = CARTESIAN_POINT ( 'NONE',  ( 40.45084971874737079, 26.98125000068279888, -29.38926261462366440 ) ) ;
#4719 = VECTOR ( 'NONE', #2837, 1000.000000000000000 ) ;
#4721 = ORIENTED_EDGE ( 'NONE', *, *, #14864, .F. ) ;
#4722 = CARTESIAN_POINT ( 'NONE',  ( -7.919222016226816763, 35.55125428154684641, -49.99999999999999289 ) ) ;
#4723 = CARTESIAN_POINT ( 'NONE',  ( 40.34137639590981905, 38.72187500034139873, 29.30972558990010768 ) ) ;
#4724 = CARTESIAN_POINT ( 'NONE',  ( -49.86468353124999453, 46.02187500034140299, 16.20201782572377525 ) ) ;
#4725 = CARTESIAN_POINT ( 'NONE',  ( 50.00000000000000000, 41.00000000000000000, -6.123233995736766085E-15 ) ) ;
#4726 = CARTESIAN_POINT ( 'NONE',  ( 49.86468353125001585, 20.82187500034140015, 16.20201782572375038 ) ) ;
#4727 = AXIS2_PLACEMENT_3D ( 'NONE', #11884, #4326, #4073 ) ;
#4728 = APPLICATION_PROTOCOL_DEFINITION ( 'draft international standard', 'automotive_design', 1998, #10053 ) ;
#4729 = CARTESIAN_POINT ( 'NONE',  ( -49.99999999999999289, 35.68125000068278752, -16.24598481164531449 ) ) ;
#4730 = AXIS2_PLACEMENT_3D ( 'NONE', #7216, #3556, #878 ) ;
#4731 = CARTESIAN_POINT ( 'NONE',  ( -30.81806926056963292, 37.62187500034139020, -42.41743335407647209 ) ) ;
#4732 = CARTESIAN_POINT ( 'NONE',  ( -27.61612561546114009, 282.5087415087664908, -10.11612561546113298 ) ) ;
#4733 = VERTEX_POINT ( 'NONE', #4608 ) ;
#4734 = ADVANCED_FACE ( 'NONE', ( #7109 ), #7019, .T. ) ;
#4735 = CARTESIAN_POINT ( 'NONE',  ( 30.81806926056964002, 34.62187500034139731, 42.41743335407647209 ) ) ;
#4736 = PLANE ( 'NONE',  #9457 ) ;
#4737 = EDGE_LOOP ( 'NONE', ( #5049, #16013, #12238, #8926 ) ) ;
#4738 = ORIENTED_EDGE ( 'NONE', *, *, #147, .F. ) ;
#4739 = ORIENTED_EDGE ( 'NONE', *, *, #5282, .F. ) ;
#4740 = DIRECTION ( 'NONE',  ( -1.156482317317871478E-16, 0.000000000000000000, -1.000000000000000000 ) ) ;
#4741 = DIRECTION ( 'NONE',  ( -0.000000000000000000, -0.000000000000000000, -1.000000000000000000 ) ) ;
#4742 = FACE_OUTER_BOUND ( 'NONE', #14988, .T. ) ;
#4743 = CARTESIAN_POINT ( 'NONE',  ( 15.45084971874737789, 20.60000000000000142, 47.55282581475767500 ) ) ;
#4744 = CARTESIAN_POINT ( 'NONE',  ( 15.40903463028482356, 36.45937500034139589, 47.42413220539093999 ) ) ;
#4745 = CARTESIAN_POINT ( 'NONE',  ( 49.86468353125000164, 48.85937500034139447, -6.106662507704105588E-15 ) ) ;
#4746 = CARTESIAN_POINT ( 'NONE',  ( -3.111920190527341144E-15, 25.50000000000000355, -50.00000000000000000 ) ) ;
#4747 = CARTESIAN_POINT ( 'NONE',  ( -40.34137639590981905, 49.72187500034139873, -29.30972558990011478 ) ) ;
#4748 = DIRECTION ( 'NONE',  ( 6.938893903907231459E-18, -1.000000000000000000, -5.551115123125782702E-17 ) ) ;
#4749 = LINE ( 'NONE', #14684, #6575 ) ;
#4750 = CARTESIAN_POINT ( 'NONE',  ( -7.919222016226934890, 34.44874571845316069, 49.99999999999996447 ) ) ;
#4751 = EDGE_CURVE ( 'NONE', #3156, #7423, #1762, .T. ) ;
#4752 =( NAMED_UNIT ( * ) SI_UNIT ( $, .STERADIAN. ) SOLID_ANGLE_UNIT ( ) );
#4753 = ORIENTED_EDGE ( 'NONE', *, *, #10033, .T. ) ;
#4754 = CARTESIAN_POINT ( 'NONE',  ( 15.40903463028482356, 30.45937500034139589, 47.42413220539093999 ) ) ;
#4755 = DIRECTION ( 'NONE',  ( 0.000000000000000000, 0.000000000000000000, -1.000000000000000000 ) ) ;
#4756 = ORIENTED_EDGE ( 'NONE', *, *, #15914, .F. ) ;
#4757 = ORIENTED_EDGE ( 'NONE', *, *, #3754, .F. ) ;
#4758 = CARTESIAN_POINT ( 'NONE',  ( 49.99999999999999289, 42.88125000068278325, -16.24598481164532160 ) ) ;
#4759 = FACE_OUTER_BOUND ( 'NONE', #13729, .T. ) ;
#4760 = CARTESIAN_POINT ( 'NONE',  ( 8.446640517145639571E-15, 28.49999999999999645, 50.00000000000000000 ) ) ;
#4761 = ORIENTED_EDGE ( 'NONE', *, *, #4751, .F. ) ;
#4762 = FACE_OUTER_BOUND ( 'NONE', #12008, .T. ) ;
#4763 = CARTESIAN_POINT ( 'NONE',  ( -50.00000000000000000, 27.78125000068279959, 0.000000000000000000 ) ) ;
#4764 = CARTESIAN_POINT ( 'NONE',  ( 1.235979693235591175E-19, 4.999999999999997335, 99.11836509645767990 ) ) ;
#4765 = FACE_OUTER_BOUND ( 'NONE', #10137, .T. ) ;
#4766 = FACE_OUTER_BOUND ( 'NONE', #12852, .T. ) ;
#4767 = PLANE ( 'NONE',  #2892 ) ;
#4768 = DIRECTION ( 'NONE',  ( -1.000000000000000000, 0.000000000000000000, 0.000000000000000000 ) ) ;
#4769 = CARTESIAN_POINT ( 'NONE',  ( 30.27664397204019409, 25.00000000000000355, -26.14048258526078072 ) ) ;
#4770 = CARTESIAN_POINT ( 'NONE',  ( 0.000000000000000000, 274.0000000000000000, 0.000000000000000000 ) ) ;
#4771 = CARTESIAN_POINT ( 'NONE',  ( 50.00000000000000000, 44.78125000068280315, -6.123233995736766085E-15 ) ) ;
#4772 = PLANE ( 'NONE',  #2846 ) ;
#4773 = CARTESIAN_POINT ( 'NONE',  ( 9.657523855033129090E-15, 26.50000000000000355, 52.57311121191334990 ) ) ;
#4774 = DIRECTION ( 'NONE',  ( 0.000000000000000000, 0.000000000000000000, 1.000000000000000000 ) ) ;
#4775 = CARTESIAN_POINT ( 'NONE',  ( -40.45084971874737789, 43.80000000000000426, -29.38926261462365730 ) ) ;
#4776 = CARTESIAN_POINT ( 'NONE',  ( 0.000000000000000000, 22.50000000000000000, 101.0000000000000000 ) ) ;
#4777 = ORIENTED_EDGE ( 'NONE', *, *, #2394, .F. ) ;
#4778 = DIRECTION ( 'NONE',  ( 0.000000000000000000, 0.7071067811865487940, -0.7071067811865463515 ) ) ;
#4779 = EDGE_LOOP ( 'NONE', ( #11743, #16056, #16210, #15253, #5887 ) ) ;
#4780 = DIRECTION ( 'NONE',  ( 0.9945218953682730678, 0.1045284632676572317, 0.000000000000000000 ) ) ;
#4781 = CARTESIAN_POINT ( 'NONE',  ( 49.86468353125001585, 36.75937500034138594, 16.20201782572375038 ) ) ;
#4782 = EDGE_CURVE ( 'NONE', #4820, #14671, #6827, .T. ) ;
#4783 = CARTESIAN_POINT ( 'NONE',  ( 14.32166083077716578, 13.65403499491884354, 101.6666710451724214 ) ) ;
#4784 = LINE ( 'NONE', #11092, #10775 ) ;
#4785 = CARTESIAN_POINT ( 'NONE',  ( 3.750000000000036859, 40.00000000000000711, 6.495190528383278483 ) ) ;
#4786 =( BOUNDED_CURVE ( )  B_SPLINE_CURVE ( 3, ( #6243, #13954, #12797, #8808 ),
 .UNSPECIFIED., .F., .T. ) 
 B_SPLINE_CURVE_WITH_KNOTS ( ( 4, 4 ),
 ( 4.523772594209285458, 4.901005366560093890 ),
 .UNSPECIFIED. ) 
 CURVE ( )  GEOMETRIC_REPRESENTATION_ITEM ( )  RATIONAL_B_SPLINE_CURVE ( ( 1.000000000000000000, 0.9881764018959044993, 0.9881764018959044993, 1.000000000000000000 ) ) 
 REPRESENTATION_ITEM ( '' )  );
#4787 = DIRECTION ( 'NONE',  ( -5.069245582283711292E-17, -1.000000000000000000, 8.780190904559502465E-17 ) ) ;
#4788 = VECTOR ( 'NONE', #6561, 1000.000000000000000 ) ;
#4789 = CARTESIAN_POINT ( 'NONE',  ( -15.40903463028481646, 27.52187500034139944, -47.42413220539093999 ) ) ;
#4790 = CARTESIAN_POINT ( 'NONE',  ( -40.34137639590981905, 31.65937500034139873, -29.30972558990011478 ) ) ;
#4791 = CARTESIAN_POINT ( 'NONE',  ( 6.661118525004998681, 38.69041383028350367, 101.0000000000000000 ) ) ;
#4792 = CARTESIAN_POINT ( 'NONE',  ( 15.40903463028482356, 36.52187500034139589, 47.42413220539093999 ) ) ;
#4793 = DIRECTION ( 'NONE',  ( 0.3535533905932685128, -0.7071067811865462405, -0.6123724356957990222 ) ) ;
#4794 = CARTESIAN_POINT ( 'NONE',  ( 15.40903463028482356, 44.45937500034139589, 47.42413220539093999 ) ) ;
#4795 = CARTESIAN_POINT ( 'NONE',  ( 30.81806926056962936, 37.22187500034139873, -42.41743335407647209 ) ) ;
#4796 = CARTESIAN_POINT ( 'NONE',  ( -40.45084971874737079, 46.20000000000000284, 29.38926261462367151 ) ) ;
#4797 = EDGE_CURVE ( 'NONE', #2646, #7011, #11180, .T. ) ;
#4798 = B_SPLINE_CURVE_WITH_KNOTS ( 'NONE', 3,
 ( #3063, #9235, #15697, #9143 ),
 .UNSPECIFIED., .F., .F.,
 ( 4, 4 ),
 ( 2.829004760700636057E-07, 0.001414802801989368088 ),
 .UNSPECIFIED. ) ;
#4799 = ORIENTED_EDGE ( 'NONE', *, *, #9262, .F. ) ;
#4800 = AXIS2_PLACEMENT_3D ( 'NONE', #7481, #5168, #11466 ) ;
#4801 = CARTESIAN_POINT ( 'NONE',  ( -30.81806926056963292, 41.55937500034139731, -42.41743335407646498 ) ) ;
#4802 = ORIENTED_EDGE ( 'NONE', *, *, #14156, .F. ) ;
#4803 = CARTESIAN_POINT ( 'NONE',  ( -30.90169943749474868, 23.48125000068279888, -42.53254041760200721 ) ) ;
#4804 = ORIENTED_EDGE ( 'NONE', *, *, #3372, .T. ) ;
#4805 = DIRECTION ( 'NONE',  ( 0.000000000000000000, 0.000000000000000000, 1.000000000000000000 ) ) ;
#4806 = CARTESIAN_POINT ( 'NONE',  ( -49.86468353124999453, 36.02187500034139589, 16.20201782572377169 ) ) ;
#4807 = CARTESIAN_POINT ( 'NONE',  ( 49.86468353124999453, 49.02187500034140299, -16.20201782572376459 ) ) ;
#4808 = CARTESIAN_POINT ( 'NONE',  ( 15.45084971874736723, 31.39999999999999858, -47.55282581475768211 ) ) ;
#4809 = EDGE_CURVE ( 'NONE', #11650, #4712, #12105, .T. ) ;
#4810 = CARTESIAN_POINT ( 'NONE',  ( 49.86468353124999453, 25.02187500034139589, -16.20201782572376459 ) ) ;
#4811 = CARTESIAN_POINT ( 'NONE',  ( -49.99999999999999289, 33.88125000068280457, 16.24598481164533226 ) ) ;
#4812 = CARTESIAN_POINT ( 'NONE',  ( -30.81806926056963292, 39.62187500034138310, -42.41743335407647209 ) ) ;
#4813 = CARTESIAN_POINT ( 'NONE',  ( -30.00000000000000711, 282.0000000000000000, -12.49999999999999822 ) ) ;
#4814 = ORIENTED_EDGE ( 'NONE', *, *, #8129, .T. ) ;
#4815 = CARTESIAN_POINT ( 'NONE',  ( -49.86468353124999453, 35.82187500034139305, -16.20201782572375393 ) ) ;
#4816 = CARTESIAN_POINT ( 'NONE',  ( -15.45084971874737256, 43.38125000068279746, -47.55282581475767500 ) ) ;
#4817 = VERTEX_POINT ( 'NONE', #12164 ) ;
#4818 = ORIENTED_EDGE ( 'NONE', *, *, #13824, .T. ) ;
#4819 = EDGE_CURVE ( 'NONE', #15674, #12352, #15456, .T. ) ;
#4820 = VERTEX_POINT ( 'NONE', #6025 ) ;
#4821 = CARTESIAN_POINT ( 'NONE',  ( 0.000000000000000000, 20.00000000000000355, 0.000000000000000000 ) ) ;
#4822 = LINE ( 'NONE', #12361, #1461 ) ;
#4823 = CARTESIAN_POINT ( 'NONE',  ( -15.45084971874737256, 23.38125000068280102, -47.55282581475767500 ) ) ;
#4824 = CARTESIAN_POINT ( 'NONE',  ( -15.40903463028481646, 37.45937500034139589, -47.42413220539093999 ) ) ;
#4825 = CARTESIAN_POINT ( 'NONE',  ( 49.86468353125000164, 42.85937500034140157, -6.106662507704105588E-15 ) ) ;
#4826 = CARTESIAN_POINT ( 'NONE',  ( 30.90169943749475223, 24.69999999999999929, 42.53254041760199300 ) ) ;
#4827 = CARTESIAN_POINT ( 'NONE',  ( 0.000000000000000000, 22.50000000000000000, 102.0000000000000142 ) ) ;
#4828 = FILL_AREA_STYLE ('',( #13533 ) ) ;
#4829 = CARTESIAN_POINT ( 'NONE',  ( -50.00000000000000000, 40.00000000000000000, 0.000000000000000000 ) ) ;
#4830 = CARTESIAN_POINT ( 'NONE',  ( 7.919222016226809657, 43.22999571913594963, -50.00000000000000000 ) ) ;
#4831 = ORIENTED_EDGE ( 'NONE', *, *, #1924, .F. ) ;
#4832 = CARTESIAN_POINT ( 'NONE',  ( -40.34137639590981195, 26.05937500034139731, 29.30972558990012189 ) ) ;
#4833 = EDGE_LOOP ( 'NONE', ( #5425, #13001, #1897, #4124 ) ) ;
#4834 = EDGE_LOOP ( 'NONE', ( #11539, #16034, #16189, #7982 ) ) ;
#4835 = VERTEX_POINT ( 'NONE', #15982 ) ;
#4836 = ADVANCED_FACE ( 'NONE', ( #5776 ), #14721, .T. ) ;
#4837 = ADVANCED_FACE ( 'NONE', ( #15906 ), #4530, .T. ) ;
#4838 = CARTESIAN_POINT ( 'NONE',  ( 50.00000000000000711, 40.68125000068280173, 16.24598481164530739 ) ) ;
#4839 = CARTESIAN_POINT ( 'NONE',  ( 0.5000000000000000000, 242.0000000000000284, -47.99999999999999289 ) ) ;
#4840 = FILL_AREA_STYLE ('',( #3577 ) ) ;
#4841 = VERTEX_POINT ( 'NONE', #10920 ) ;
#4842 = CARTESIAN_POINT ( 'NONE',  ( -15.45084971874736368, 48.18125000068280173, 47.55282581475768211 ) ) ;
#4843 = CARTESIAN_POINT ( 'NONE',  ( -40.45084971874737079, 27.98125000068279888, 29.38926261462367151 ) ) ;
#4844 = DIRECTION ( 'NONE',  ( 0.2079116908177531531, 0.9781476007338069101, 0.000000000000000000 ) ) ;
#4845 = FACE_OUTER_BOUND ( 'NONE', #10162, .T. ) ;
#4846 = CARTESIAN_POINT ( 'NONE',  ( 49.99999999999999289, 26.88125000068280102, -16.24598481164532160 ) ) ;
#4847 = LINE ( 'NONE', #906, #5029 ) ;
#4848 = CARTESIAN_POINT ( 'NONE',  ( 0.000000000000000000, 193.4213562373095385, 0.000000000000000000 ) ) ;
#4849 = LINE ( 'NONE', #4769, #2200 ) ;
#4850 = DIRECTION ( 'NONE',  ( 0.000000000000000000, 0.000000000000000000, 1.000000000000000000 ) ) ;
#4851 = CARTESIAN_POINT ( 'NONE',  ( -30.90169943749474868, 45.48125000068279178, -42.53254041760200721 ) ) ;
#4852 = DIRECTION ( 'NONE',  ( -1.000000000000000000, 0.000000000000000000, 0.000000000000000000 ) ) ;
#4853 = CARTESIAN_POINT ( 'NONE',  ( -30.90169943749474868, 29.70000000000000284, -42.53254041760200721 ) ) ;
#4854 = CARTESIAN_POINT ( 'NONE',  ( -15.45084971874736368, 26.40000000000000213, 47.55282581475768211 ) ) ;
#4855 = CARTESIAN_POINT ( 'NONE',  ( -50.00000000000000000, 41.78125000068280315, 0.000000000000000000 ) ) ;
#4856 = EDGE_CURVE ( 'NONE', #1228, #5387, #2173, .T. ) ;
#4857 = CARTESIAN_POINT ( 'NONE',  ( 15.40903463028481113, 45.25937500034140015, -47.42413220539094709 ) ) ;
#4858 = EDGE_CURVE ( 'NONE', #243, #15421, #1217, .T. ) ;
#4859 = ORIENTED_EDGE ( 'NONE', *, *, #7453, .F. ) ;
#4860 = CARTESIAN_POINT ( 'NONE',  ( -30.00000000000000711, 282.0000000000000000, -12.49999999999999822 ) ) ;
#4861 = ORIENTED_EDGE ( 'NONE', *, *, #815, .F. ) ;
#4862 = CARTESIAN_POINT ( 'NONE',  ( 7.919222016226818539, 49.44874571845315359, -50.00000000000000000 ) ) ;
#4863 = CARTESIAN_POINT ( 'NONE',  ( 9.631387414534489405E-15, 36.35937500034140157, 52.43083105670540789 ) ) ;
#4864 = EDGE_CURVE ( 'NONE', #10616, #16078, #5746, .T. ) ;
#4865 = CARTESIAN_POINT ( 'NONE',  ( -15.40544456622763470, 14.18301270189214947, 102.0000000000000142 ) ) ;
#4866 = CARTESIAN_POINT ( 'NONE',  ( -6.658212670116278709, 38.68388717334321569, 101.0000000000000000 ) ) ;
#4867 = CARTESIAN_POINT ( 'NONE',  ( -3.111920190527341144E-15, 35.50000000000000000, -50.00000000000000000 ) ) ;
#4868 = CARTESIAN_POINT ( 'NONE',  ( 15.45084971874737789, 44.38125000068279746, 47.55282581475767500 ) ) ;
#4869 = CARTESIAN_POINT ( 'NONE',  ( 15.40903463028482356, 20.52187500034139589, 47.42413220539093999 ) ) ;
#4870 = CARTESIAN_POINT ( 'NONE',  ( 49.86468353125000164, 26.85937500034139802, -6.106662507704105588E-15 ) ) ;
#4871 = CARTESIAN_POINT ( 'NONE',  ( -15.45084971874737256, 35.60000000000000142, -47.55282581475767500 ) ) ;
#4872 = CARTESIAN_POINT ( 'NONE',  ( -49.86468353125000164, 37.92187500034140157, 0.000000000000000000 ) ) ;
#4873 = DIRECTION ( 'NONE',  ( -0.000000000000000000, -1.000000000000000000, -0.000000000000000000 ) ) ;
#4874 = CARTESIAN_POINT ( 'NONE',  ( 40.34137639590981195, 41.05937500034139731, -29.30972558990011834 ) ) ;
#4875 = CARTESIAN_POINT ( 'NONE',  ( 30.81806926056964002, 38.62187500034139731, 42.41743335407647209 ) ) ;
#4876 = CARTESIAN_POINT ( 'NONE',  ( -40.45084971874737079, 48.20000000000000284, 29.38926261462367151 ) ) ;
#4877 = VERTEX_POINT ( 'NONE', #3606 ) ;
#4878 = CARTESIAN_POINT ( 'NONE',  ( 49.86468353125000164, 44.85937500034140157, -6.106662507704105588E-15 ) ) ;
#4879 = ORIENTED_EDGE ( 'NONE', *, *, #3752, .F. ) ;
#4881 =( BOUNDED_CURVE ( )  B_SPLINE_CURVE ( 2, ( #14442, #13130, #11885, #15700, #6983, #10810, #7899, #4169, #560, #9238, #14291, #2913, #12038 ),
 .UNSPECIFIED., .F., .T. ) 
 B_SPLINE_CURVE_WITH_KNOTS ( ( 3, 2, 2, 2, 2, 2, 3 ),
 ( 0.8833333333333334147, 0.8866666666666667140, 0.8933333333333333126, 0.9000000000000000222, 0.9066666666666666208, 0.9133333333333333304, 0.9166666666666667407 ),
 .UNSPECIFIED. ) 
 CURVE ( )  GEOMETRIC_REPRESENTATION_ITEM ( )  RATIONAL_B_SPLINE_CURVE ( ( 0.9755282581475768211, 0.9755282581475771542, 1.000000000000000000, 0.9510565162951535312, 1.000000000000000000, 0.9510565162951535312, 1.000000000000000000, 0.9510565162951535312, 1.000000000000000000, 0.9510565162951535312, 1.000000000000000000, 0.9755282581475763770, 0.9755282581475768211 ) ) 
 REPRESENTATION_ITEM ( '' )  );
#4880 = CARTESIAN_POINT ( 'NONE',  ( 30.90169943749474157, 23.08125000068279320, -42.53254041760200721 ) ) ;
#4882 = CARTESIAN_POINT ( 'NONE',  ( -15.45084971874736368, 34.39999999999999858, 47.55282581475768211 ) ) ;
#4883 = VECTOR ( 'NONE', #6935, 999.9999999999998863 ) ;
#4884 = CARTESIAN_POINT ( 'NONE',  ( -7.919222016226870942, 36.44874571845315359, 49.99999999999997158 ) ) ;
#4885 = CARTESIAN_POINT ( 'NONE',  ( -49.86468353125000164, 41.92187500034139447, 0.000000000000000000 ) ) ;
#4886 = DIRECTION ( 'NONE',  ( 0.9781476007338042455, 0.2079116908177664758, 0.000000000000000000 ) ) ;
#4887 = CARTESIAN_POINT ( 'NONE',  ( 40.34137639590981195, 21.12187500034139376, -29.30972558990011834 ) ) ;
#4888 = CARTESIAN_POINT ( 'NONE',  ( 30.90169943749474157, 27.08125000068280031, -42.53254041760200721 ) ) ;
#4889 = CARTESIAN_POINT ( 'NONE',  ( 15.40903463028481113, 37.32187500034140015, -47.42413220539094709 ) ) ;
#4890 = CARTESIAN_POINT ( 'NONE',  ( -24.81239020281865137, 286.7275190727449967, -7.312390202818956908 ) ) ;
#4891 = CARTESIAN_POINT ( 'NONE',  ( 49.86468353124999453, 35.02187500034139589, -16.20201782572376459 ) ) ;
#4892 = CARTESIAN_POINT ( 'NONE',  ( -2.547328955960238000E-13, 32.28125000068278894, 49.99999999999999289 ) ) ;
#4893 = ORIENTED_EDGE ( 'NONE', *, *, #2451, .T. ) ;
#4894 = EDGE_LOOP ( 'NONE', ( #8044, #2276, #12130, #7281 ) ) ;
#4895 = ADVANCED_FACE ( 'NONE', ( #6183 ), #14978, .T. ) ;
#4896 = VERTEX_POINT ( 'NONE', #3768 ) ;
#4897 = CARTESIAN_POINT ( 'NONE',  ( -8.660254037844387298, 20.00000000000000355, 5.000000000000000000 ) ) ;
#4898 = CARTESIAN_POINT ( 'NONE',  ( 0.000000000000000000, 262.0000000000000000, 79.49773270518484480 ) ) ;
#4899 = CYLINDRICAL_SURFACE ( 'NONE', #2278, 50.00000000000000000 ) ;
#4900 = FACE_OUTER_BOUND ( 'NONE', #12337, .T. ) ;
#4901 = CARTESIAN_POINT ( 'NONE',  ( 15.40903463028481113, 35.25937500034139305, -47.42413220539094709 ) ) ;
#4902 = CARTESIAN_POINT ( 'NONE',  ( 40.34137639590981905, 40.65937500034139873, 29.30972558990010768 ) ) ;
#4903 = AXIS2_PLACEMENT_3D ( 'NONE', #4770, #12059, #4850 ) ;
#4904 = DIRECTION ( 'NONE',  ( 0.000000000000000000, -1.000000000000000000, 0.000000000000000000 ) ) ;
#4905 = EDGE_CURVE ( 'NONE', #12450, #4999, #13890, .T. ) ;
#4907 = EDGE_CURVE ( 'NONE', #8817, #7744, #12742, .T. ) ;
#4906 = AXIS2_PLACEMENT_3D ( 'NONE', #6167, #5018, #8895 ) ;
#4908 = DIRECTION ( 'NONE',  ( -6.938893903907231459E-18, 1.000000000000000000, 5.551115123125782702E-17 ) ) ;
#4909 = SHAPE_REPRESENTATION_RELATIONSHIP ( 'NONE' , 'NONE' ,  #5560, #1465 ) ;
#4910 = DIRECTION ( 'NONE',  ( 0.000000000000000000, 1.000000000000000000, 0.000000000000000000 ) ) ;
#4911 = CARTESIAN_POINT ( 'NONE',  ( -40.45084971874737789, 35.58125000068279320, -29.38926261462365730 ) ) ;
#4912 = EDGE_CURVE ( 'NONE', #14665, #14587, #2506, .T. ) ;
#4913 = LINE ( 'NONE', #5079, #1387 ) ;
#4914 = ORIENTED_EDGE ( 'NONE', *, *, #7088, .F. ) ;
#4915 = CARTESIAN_POINT ( 'NONE',  ( -49.86468353125000164, 25.85937500034139802, 0.000000000000000000 ) ) ;
#4916 = ORIENTED_EDGE ( 'NONE', *, *, #12556, .F. ) ;
#4917 = ORIENTED_EDGE ( 'NONE', *, *, #11691, .F. ) ;
#4918 = ORIENTED_EDGE ( 'NONE', *, *, #12310, .T. ) ;
#4919 = AXIS2_PLACEMENT_3D ( 'NONE', #2942, #11751, #10348 ) ;
#4920 = EDGE_CURVE ( 'NONE', #13519, #7011, #12188, .T. ) ;
#4921 = CARTESIAN_POINT ( 'NONE',  ( -15.45084971874737256, 35.38125000068279746, -47.55282581475767500 ) ) ;
#4922 = DIRECTION ( 'NONE',  ( -0.3535533905932715104, 0.7071067811865487940, 0.6123724356957942483 ) ) ;
#4923 = DIRECTION ( 'NONE',  ( -0.000000000000000000, -1.000000000000000000, -0.000000000000000000 ) ) ;
#4924 = ORIENTED_EDGE ( 'NONE', *, *, #9988, .T. ) ;
#4925 = DIRECTION ( 'NONE',  ( 0.000000000000000000, 0.000000000000000000, 1.000000000000000000 ) ) ;
#4926 = CARTESIAN_POINT ( 'NONE',  ( -3.407225380398804404, 31.38205016914259105, 101.0000000000000000 ) ) ;
#4927 = CARTESIAN_POINT ( 'NONE',  ( -2.902026171381852926, 5.232512297988552774, 99.03650175003853917 ) ) ;
#4928 = PLANE ( 'NONE',  #12639 ) ;
#4929 = DIRECTION ( 'NONE',  ( 1.000000000000000000, 0.000000000000000000, 0.000000000000000000 ) ) ;
#4930 = DIRECTION ( 'NONE',  ( -0.000000000000000000, -1.000000000000000000, -0.000000000000000000 ) ) ;
#4931 = DIRECTION ( 'NONE',  ( -0.000000000000000000, 1.000000000000000000, -0.000000000000000000 ) ) ;
#4932 =( NAMED_UNIT ( * ) PLANE_ANGLE_UNIT ( ) SI_UNIT ( $, .RADIAN. ) );
#4933 = DIRECTION ( 'NONE',  ( 0.000000000000000000, 0.000000000000000000, 1.000000000000000000 ) ) ;
#4934 = CARTESIAN_POINT ( 'NONE',  ( 40.45084971874737079, 48.98125000068279888, -29.38926261462366440 ) ) ;
#4935 = LINE ( 'NONE', #3751, #706 ) ;
#4936 = AXIS2_PLACEMENT_3D ( 'NONE', #13137, #15707, #4258 ) ;
#4937 = CARTESIAN_POINT ( 'NONE',  ( -49.99999999999999289, 27.89999999999999858, -16.24598481164531449 ) ) ;
#4938 = CARTESIAN_POINT ( 'NONE',  ( -40.34137639590981195, 20.05937500034139731, 29.30972558990012189 ) ) ;
#4939 = CARTESIAN_POINT ( 'NONE',  ( -15.45084971874737256, 43.60000000000000142, -47.55282581475767500 ) ) ;
#4940 = CARTESIAN_POINT ( 'NONE',  ( -40.34137639590981195, 46.05937500034139731, 29.30972558990012189 ) ) ;
#4941 = EDGE_LOOP ( 'NONE', ( #1372, #1547, #549, #12772 ) ) ;
#4942 = CARTESIAN_POINT ( 'NONE',  ( 0.000000000000000000, 22.50000000000000000, 102.0000000000000142 ) ) ;
#4943 = ORIENTED_EDGE ( 'NONE', *, *, #5027, .F. ) ;
#4944 = DIRECTION ( 'NONE',  ( -1.000000000000000000, 0.000000000000000000, 0.000000000000000000 ) ) ;
#4945 = CARTESIAN_POINT ( 'NONE',  ( 49.86468353125000164, 34.85937500034140157, -6.106662507704105588E-15 ) ) ;
#4946 = AXIS2_PLACEMENT_3D ( 'NONE', #14762, #4741, #8532 ) ;
#4947 = CARTESIAN_POINT ( 'NONE',  ( 16.48218589020105185, 28.38111794481774908, 101.0000000000000000 ) ) ;
#4948 = LINE ( 'NONE', #13264, #3881 ) ;
#4949 = CARTESIAN_POINT ( 'NONE',  ( 45.93954244148165600, 24.99999999999998579, -19.39188242381383276 ) ) ;
#4950 = CARTESIAN_POINT ( 'NONE',  ( 50.00000000000000711, 46.68125000068279462, 16.24598481164530739 ) ) ;
#4951 = CARTESIAN_POINT ( 'NONE',  ( -49.86468353124999453, 21.82187500034139305, -16.20201782572375393 ) ) ;
#4952 = CARTESIAN_POINT ( 'NONE',  ( 30.81806926056962936, 29.15937500034139518, -42.41743335407646498 ) ) ;
#4953 = CARTESIAN_POINT ( 'NONE',  ( 49.99999999999999289, 43.10000000000000142, -16.24598481164532160 ) ) ;
#4954 = CARTESIAN_POINT ( 'NONE',  ( -40.34137639590981195, 38.12187500034139731, 29.30972558990012189 ) ) ;
#4955 = CARTESIAN_POINT ( 'NONE',  ( -40.45084971874737079, 29.98125000068279888, 29.38926261462367151 ) ) ;
#4956 = CARTESIAN_POINT ( 'NONE',  ( 50.00000000000000711, 36.89999999999999858, 16.24598481164530739 ) ) ;
#4957 = CARTESIAN_POINT ( 'NONE',  ( -40.34137639590981905, 37.65937500034139873, -29.30972558990011478 ) ) ;
#4958 = AXIS2_PLACEMENT_3D ( 'NONE', #10367, #214, #12857 ) ;
#4959 = CARTESIAN_POINT ( 'NONE',  ( 30.81806926056962936, 29.22187500034139873, -42.41743335407647209 ) ) ;
#4960 = VECTOR ( 'NONE', #6023, 1000.000000000000000 ) ;
#4961 = CARTESIAN_POINT ( 'NONE',  ( 15.45084971874736723, 45.40000000000000568, -47.55282581475768211 ) ) ;
#4962 = EDGE_CURVE ( 'NONE', #13481, #15793, #13880, .T. ) ;
#4963 = ORIENTED_EDGE ( 'NONE', *, *, #10194, .F. ) ;
#4964 = CARTESIAN_POINT ( 'NONE',  ( 15.40903463028482356, 40.45937500034139589, 47.42413220539093999 ) ) ;
#4965 = EDGE_LOOP ( 'NONE', ( #740, #12195, #4756 ) ) ;
#4966 = CARTESIAN_POINT ( 'NONE',  ( 50.00000000000000000, 24.78125000068279959, -6.123233995736766085E-15 ) ) ;
#4967 = CLOSED_SHELL ( 'NONE', ( #4133, #11945, #9888, #2535, #9968, #7240, #4497, #11822, #12516, #9974, #9380, #13799, #907, #14274, #71, #2489, #5802, #5210, #8839, #3205, #916, #8610, #11903, #506, #4079, #16402, #11304, #8143, #529, #3423, #12587, #8990, #9356, #2069, #460, #14023, #8211, #2641, #15494, #7086 ) ) ;
#4968 = PLANE ( 'NONE',  #2505 ) ;
#4969 = CIRCLE ( 'NONE', #13182, 16.50000000000000711 ) ;
#4970 = CARTESIAN_POINT ( 'NONE',  ( 15.40903463028482356, 22.52187500034139589, 47.42413220539093999 ) ) ;
#4971 = VECTOR ( 'NONE', #7808, 1000.000000000000000 ) ;
#4972 = FACE_OUTER_BOUND ( 'NONE', #1040, .T. ) ;
#4973 = CARTESIAN_POINT ( 'NONE',  ( -15.40903463028480580, 40.32187500034140015, 47.42413220539094709 ) ) ;
#4974 = DIRECTION ( 'NONE',  ( 0.000000000000000000, 0.000000000000000000, 1.000000000000000000 ) ) ;
#4975 = CARTESIAN_POINT ( 'NONE',  ( -15.45084971874737256, 49.60000000000000853, -47.55282581475767500 ) ) ;
#4976 = CARTESIAN_POINT ( 'NONE',  ( -40.45084971874737789, 27.58125000068280031, -29.38926261462365730 ) ) ;
#4977 = CARTESIAN_POINT ( 'NONE',  ( -15.40903463028481646, 35.52187500034139589, -47.42413220539093999 ) ) ;
#4978 = LINE ( 'NONE', #6133, #6463 ) ;
#4979 = CIRCLE ( 'NONE', #167, 2.000000000000001776 ) ;
#4980 = CARTESIAN_POINT ( 'NONE',  ( -40.34137639590981905, 35.72187500034139163, -29.30972558990011478 ) ) ;
#4981 = CARTESIAN_POINT ( 'NONE',  ( -7.919222016226934890, 32.22999571913595673, 49.99999999999996447 ) ) ;
#4982 = VERTEX_POINT ( 'NONE', #13977 ) ;
#4983 = EDGE_LOOP ( 'NONE', ( #8353, #209, #490, #453 ) ) ;
#4984 = DIRECTION ( 'NONE',  ( 0.000000000000000000, 0.000000000000000000, -1.000000000000000000 ) ) ;
#4985 = CYLINDRICAL_SURFACE ( 'NONE', #8099, 5.000000000000000888 ) ;
#4986 = EDGE_CURVE ( 'NONE', #4102, #1226, #429, .T. ) ;
#4987 = PLANE ( 'NONE',  #14210 ) ;
#4988 = CARTESIAN_POINT ( 'NONE',  ( -7.919222016226934890, 24.22999571913595673, 49.99999999999996447 ) ) ;
#4989 = VECTOR ( 'NONE', #3403, 1000.000000000000000 ) ;
#4990 = EDGE_CURVE ( 'NONE', #1326, #895, #1262, .T. ) ;
#4991 = CARTESIAN_POINT ( 'NONE',  ( -30.81806926056963292, 29.55937500034139376, -42.41743335407647209 ) ) ;
#4992 = SURFACE_SIDE_STYLE ('',( #2464 ) ) ;
#4993 = AXIS2_PLACEMENT_3D ( 'NONE', #3301, #2052, #11038 ) ;
#4994 = CARTESIAN_POINT ( 'NONE',  ( -49.86468353124999453, 48.02187500034139589, 16.20201782572377169 ) ) ;
#4995 = FILL_AREA_STYLE_COLOUR ( '', #671 ) ;
#4996 = DIRECTION ( 'NONE',  ( -0.9135454576426059736, 0.4067366430757888285, 0.000000000000000000 ) ) ;
#4997 = FACE_BOUND ( 'NONE', #4411, .T. ) ;
#4998 = CARTESIAN_POINT ( 'NONE',  ( -30.90169943749474513, 41.70000000000000284, -42.53254041760200721 ) ) ;
#4999 = VERTEX_POINT ( 'NONE', #3694 ) ;
#5000 = CARTESIAN_POINT ( 'NONE',  ( -30.81806926056962226, 24.15937500034139873, 42.41743335407647919 ) ) ;
#5001 = AXIS2_PLACEMENT_3D ( 'NONE', #5654, #2829, #13215 ) ;
#5002 = VERTEX_POINT ( 'NONE', #9924 ) ;
#5003 = ORIENTED_EDGE ( 'NONE', *, *, #4986, .T. ) ;
#5004 = EDGE_CURVE ( 'NONE', #15357, #9775, #15592, .T. ) ;
#5005 = ORIENTED_EDGE ( 'NONE', *, *, #6590, .F. ) ;
#5006 = VERTEX_POINT ( 'NONE', #5037 ) ;
#5007 = CARTESIAN_POINT ( 'NONE',  ( -49.99999999999999289, 37.68125000068278752, -16.24598481164531449 ) ) ;
#5008 = FACE_OUTER_BOUND ( 'NONE', #7985, .T. ) ;
#5009 = LINE ( 'NONE', #5087, #13407 ) ;
#5010 = VERTEX_POINT ( 'NONE', #10091 ) ;
#5011 = CARTESIAN_POINT ( 'NONE',  ( 49.99999999999999289, 38.88125000068279036, -16.24598481164532160 ) ) ;
#5012 = DIRECTION ( 'NONE',  ( 0.000000000000000000, 0.000000000000000000, 1.000000000000000000 ) ) ;
#5013 = CARTESIAN_POINT ( 'NONE',  ( 40.34137639590981905, 48.65937500034139873, 29.30972558990010768 ) ) ;
#5014 = PLANE ( 'NONE',  #14232 ) ;
#5015 = LINE ( 'NONE', #1318, #7534 ) ;
#5016 = FACE_OUTER_BOUND ( 'NONE', #5518, .T. ) ;
#5017 = DIRECTION ( 'NONE',  ( -0.000000000000000000, 0.000000000000000000, 1.000000000000000000 ) ) ;
#5018 = DIRECTION ( 'NONE',  ( -0.000000000000000000, -1.000000000000000000, -0.000000000000000000 ) ) ;
#5019 = CARTESIAN_POINT ( 'NONE',  ( 40.45084971874737789, 46.58125000068280031, 29.38926261462365375 ) ) ;
#5020 = CARTESIAN_POINT ( 'NONE',  ( 40.45084971874737079, 21.19999999999999929, -29.38926261462366440 ) ) ;
#5021 = EDGE_CURVE ( 'NONE', #5355, #172, #13702, .T. ) ;
#5022 = CARTESIAN_POINT ( 'NONE',  ( 49.99999999999999289, 21.09999999999999787, -16.24598481164532160 ) ) ;
#5023 = DIRECTION ( 'NONE',  ( -0.000000000000000000, -1.000000000000000000, -0.000000000000000000 ) ) ;
#5024 = CARTESIAN_POINT ( 'NONE',  ( -49.99999999999999289, 44.09999999999999432, 16.24598481164533226 ) ) ;
#5025 = CARTESIAN_POINT ( 'NONE',  ( -3.210462471511496205E-15, 45.35937500034139447, -52.43083105670540789 ) ) ;
#5026 = ORIENTED_EDGE ( 'NONE', *, *, #5316, .F. ) ;
#5027 = EDGE_CURVE ( 'NONE', #7197, #7494, #11, .T. ) ;
#5028 = CARTESIAN_POINT ( 'NONE',  ( 4.898587196589413026E-15, 32.49999999999999289, 40.00000000000000000 ) ) ;
#5029 = VECTOR ( 'NONE', #8402, 1000.000000000000000 ) ;
#5030 = ORIENTED_EDGE ( 'NONE', *, *, #5371, .T. ) ;
#5031 = DIRECTION ( 'NONE',  ( 0.000000000000000000, 0.000000000000000000, 1.000000000000000000 ) ) ;
#5032 = CARTESIAN_POINT ( 'NONE',  ( 40.34137639590981905, 28.65937500034139873, 29.30972558990010768 ) ) ;
#5033 = EDGE_CURVE ( 'NONE', #11588, #16127, #820, .T. ) ;
#5034 = CARTESIAN_POINT ( 'NONE',  ( -37.77664397204053159, 40.00000000000000711, -13.15010152849376190 ) ) ;
#5035 = DIRECTION ( 'NONE',  ( 0.000000000000000000, 0.000000000000000000, -1.000000000000000000 ) ) ;
#5036 = CARTESIAN_POINT ( 'NONE',  ( 45.33038492356498494, 25.00000000000000000, -20.77601661419118173 ) ) ;
#5037 = CARTESIAN_POINT ( 'NONE',  ( 5.510910596163090344E-15, 262.0000000000000000, 45.00000000000000711 ) ) ;
#5038 = CARTESIAN_POINT ( 'NONE',  ( 49.86468353125001585, 24.82187500034139305, 16.20201782572375038 ) ) ;
#5039 = CARTESIAN_POINT ( 'NONE',  ( -40.34137639590981905, 23.65937500034139518, -29.30972558990011478 ) ) ;
#5040 = CARTESIAN_POINT ( 'NONE',  ( 2.600676159226421000E-13, 31.28125000068279604, -49.99999999999999289 ) ) ;
#5041 = CARTESIAN_POINT ( 'NONE',  ( -40.34137639590981905, 33.72187500034139873, -29.30972558990011478 ) ) ;
#5042 = CARTESIAN_POINT ( 'NONE',  ( 0.000000000000000000, 247.0000000000000284, 0.000000000000000000 ) ) ;
#5043 = CIRCLE ( 'NONE', #12460, 16.50000000000000711 ) ;
#5044 = CARTESIAN_POINT ( 'NONE',  ( -15.45084971874736368, 32.39999999999999858, 47.55282581475768211 ) ) ;
#5045 = CARTESIAN_POINT ( 'NONE',  ( 9.631387414534489405E-15, 38.35937500034139447, 52.43083105670540789 ) ) ;
#5046 = CARTESIAN_POINT ( 'NONE',  ( 30.81806926056964002, 28.62187500034140086, 42.41743335407647209 ) ) ;
#5047 = CARTESIAN_POINT ( 'NONE',  ( 50.00000000000000000, 47.00000000000000000, -6.123233995736766085E-15 ) ) ;
#5048 = B_SPLINE_CURVE_WITH_KNOTS ( 'NONE', 3,
 ( #14963, #15126, #7489, #2411 ),
 .UNSPECIFIED., .F., .F.,
 ( 4, 4 ),
 ( 2.829004760659353259E-07, 0.001414802801989363968 ),
 .UNSPECIFIED. ) ;
#5049 = ORIENTED_EDGE ( 'NONE', *, *, #16166, .F. ) ;
#5050 = CARTESIAN_POINT ( 'NONE',  ( -40.34137639590981195, 38.05937500034139731, 29.30972558990012189 ) ) ;
#5051 = ORIENTED_EDGE ( 'NONE', *, *, #9009, .F. ) ;
#5052 = ORIENTED_EDGE ( 'NONE', *, *, #11589, .T. ) ;
#5053 = EDGE_CURVE ( 'NONE', #15026, #14824, #3004, .T. ) ;
#5054 = CARTESIAN_POINT ( 'NONE',  ( 19.99999999999659650, 286.6727470533784867, -7.500000000000000888 ) ) ;
#5055 = CARTESIAN_POINT ( 'NONE',  ( 30.90169943749475578, 20.48125000068279178, 42.53254041760200010 ) ) ;
#5056 = VECTOR ( 'NONE', #10048, 1000.000000000000000 ) ;
#5057 = DIRECTION ( 'NONE',  ( 0.000000000000000000, -1.000000000000000000, 0.000000000000000000 ) ) ;
#5058 = CARTESIAN_POINT ( 'NONE',  ( -40.34137639590981195, 22.12187500034139731, 29.30972558990012189 ) ) ;
#5059 = CARTESIAN_POINT ( 'NONE',  ( 7.580410092413998768, 102.0000000000000142, -5.000000000000000000 ) ) ;
#5060 = CARTESIAN_POINT ( 'NONE',  ( -3.210462471511496205E-15, 41.42187500034140157, -52.43083105670540789 ) ) ;
#5061 = CARTESIAN_POINT ( 'NONE',  ( 0.000000000000000000, 262.0000000000000000, 0.000000000000000000 ) ) ;
#5062 = CARTESIAN_POINT ( 'NONE',  ( -15.45084971874737256, 45.60000000000000142, -47.55282581475767500 ) ) ;
#5063 = CARTESIAN_POINT ( 'NONE',  ( 30.90169943749475578, 30.48125000068279533, 42.53254041760200010 ) ) ;
#5064 = CARTESIAN_POINT ( 'NONE',  ( 49.86468353125001585, 48.82187500034139305, 16.20201782572375038 ) ) ;
#5065 = CARTESIAN_POINT ( 'NONE',  ( 49.86468353125000164, 36.92187500034140157, -6.106662507704105588E-15 ) ) ;
#5066 = DIRECTION ( 'NONE',  ( -0.000000000000000000, -1.000000000000000000, -0.000000000000000000 ) ) ;
#5067 = CARTESIAN_POINT ( 'NONE',  ( 17.01311696148846053, 20.20909521249566154, 101.3333374614808662 ) ) ;
#5068 = EDGE_LOOP ( 'NONE', ( #14822, #4576 ) ) ;
#5069 = VERTEX_POINT ( 'NONE', #9083 ) ;
#5070 = CARTESIAN_POINT ( 'NONE',  ( -11.92169313911859341, 33.90715708214334256, 102.0000000000000142 ) ) ;
#5071 = CARTESIAN_POINT ( 'NONE',  ( 40.45084971874737789, 44.79999999999999716, 29.38926261462365375 ) ) ;
#5072 = DIRECTION ( 'NONE',  ( -0.8660254037844400399, 0.000000000000000000, -0.4999999999999976685 ) ) ;
#5073 = CARTESIAN_POINT ( 'NONE',  ( 2.600676159226420495E-13, 23.28125000068279604, -49.99999999999999289 ) ) ;
#5074 = CARTESIAN_POINT ( 'NONE',  ( -40.34137639590981195, 30.05937500034139731, 29.30972558990012189 ) ) ;
#5075 = DIRECTION ( 'NONE',  ( 2.312964634635742464E-16, 0.000000000000000000, -1.000000000000000000 ) ) ;
#5076 = CARTESIAN_POINT ( 'NONE',  ( 40.34137639590981195, 47.12187500034140442, -29.30972558990011834 ) ) ;
#5077 = FACE_OUTER_BOUND ( 'NONE', #4041, .T. ) ;
#5078 = DIRECTION ( 'NONE',  ( -1.000000000000000000, 0.000000000000000000, 0.000000000000000000 ) ) ;
#5079 = CARTESIAN_POINT ( 'NONE',  ( 5.000000000000000888, 99.08339874278649972, -0.6589959970937100397 ) ) ;
#5080 = VERTEX_POINT ( 'NONE', #421 ) ;
#5081 = CARTESIAN_POINT ( 'NONE',  ( 9.631387414534489405E-15, 26.35937500034140157, 52.43083105670540789 ) ) ;
#5082 = ORIENTED_EDGE ( 'NONE', *, *, #6849, .F. ) ;
#5083 = CARTESIAN_POINT ( 'NONE',  ( 8.446640517145639571E-15, 26.50000000000000000, 50.00000000000000000 ) ) ;
#5084 = ORIENTED_EDGE ( 'NONE', *, *, #5207, .F. ) ;
#5085 = EDGE_LOOP ( 'NONE', ( #6765, #15836, #3049, #13778 ) ) ;
#5086 = CARTESIAN_POINT ( 'NONE',  ( 0.000000000000000000, 25.00000000000000355, 0.000000000000000000 ) ) ;
#5087 = CARTESIAN_POINT ( 'NONE',  ( 6.123233995736766085E-15, 193.4213562373095385, 50.00000000000000000 ) ) ;
#5088 = CARTESIAN_POINT ( 'NONE',  ( -40.45084971874737789, 27.80000000000000071, -29.38926261462365730 ) ) ;
#5089 = CARTESIAN_POINT ( 'NONE',  ( -2.500000000000000000, 242.0000000000000284, 49.99999999999999289 ) ) ;
#5090 = CARTESIAN_POINT ( 'NONE',  ( 7.919222016226940219, 33.22999571913595673, -49.99999999999996447 ) ) ;
#5091 = DIRECTION ( 'NONE',  ( -0.5000000000000042188, -0.000000000000000000, -0.8660254037844362651 ) ) ;
#5092 = DIRECTION ( 'NONE',  ( 0.000000000000000000, 0.000000000000000000, 1.000000000000000000 ) ) ;
#5093 = DIRECTION ( 'NONE',  ( -0.8660254037844362651, 0.000000000000000000, 0.5000000000000041078 ) ) ;
#5094 =( LENGTH_UNIT ( ) NAMED_UNIT ( * ) SI_UNIT ( .MILLI., .METRE. ) );
#5095 = LINE ( 'NONE', #15200, #4361 ) ;
#5096 = CARTESIAN_POINT ( 'NONE',  ( -30.90169943749474868, 47.48125000068279178, -42.53254041760200721 ) ) ;
#5097 = CARTESIAN_POINT ( 'NONE',  ( -2.547328955960238000E-13, 20.49999999999999645, 49.99999999999999289 ) ) ;
#5098 = CARTESIAN_POINT ( 'NONE',  ( -40.45084971874737079, 22.19999999999999929, 29.38926261462367151 ) ) ;
#5099 = CARTESIAN_POINT ( 'NONE',  ( -49.86468353125000164, 19.85937500034139447, 0.000000000000000000 ) ) ;
#5100 = ORIENTED_EDGE ( 'NONE', *, *, #4713, .T. ) ;
#5101 = CARTESIAN_POINT ( 'NONE',  ( 40.34137639590981195, 47.05937500034140442, -29.30972558990011834 ) ) ;
#5102 = ORIENTED_EDGE ( 'NONE', *, *, #963, .F. ) ;
#5103 = CARTESIAN_POINT ( 'NONE',  ( -50.00000000000000000, 49.78125000068280315, 0.000000000000000000 ) ) ;
#5104 = ORIENTED_EDGE ( 'NONE', *, *, #4278, .F. ) ;
#5105 = DIRECTION ( 'NONE',  ( -0.5000000000000042188, 0.000000000000000000, -0.8660254037844361541 ) ) ;
#5106 = CARTESIAN_POINT ( 'NONE',  ( -15.40903463028481646, 27.45937500034139944, -47.42413220539093999 ) ) ;
#5107 = ADVANCED_FACE ( 'NONE', ( #8164 ), #10586, .F. ) ;
#5108 = ORIENTED_EDGE ( 'NONE', *, *, #5330, .F. ) ;
#5109 = LINE ( 'NONE', #1336, #14479 ) ;
#5110 = CARTESIAN_POINT ( 'NONE',  ( -1.157256219580996337, 39.97118149501703499, 92.94656295785023303 ) ) ;
#5111 = CARTESIAN_POINT ( 'NONE',  ( 46.73878613316200870, 24.99999999999999289, -17.37815620099810587 ) ) ;
#5112 = CARTESIAN_POINT ( 'NONE',  ( 15.40903463028482356, 34.52187500034140299, 47.42413220539093999 ) ) ;
#5113 = CARTESIAN_POINT ( 'NONE',  ( 7.919222016226827421, 47.22999571913595673, -50.00000000000000000 ) ) ;
#5114 = CARTESIAN_POINT ( 'NONE',  ( 40.34137639590981195, 25.05937500034139376, -29.30972558990011834 ) ) ;
#5115 = LINE ( 'NONE', #14062, #9212 ) ;
#5116 = CARTESIAN_POINT ( 'NONE',  ( -30.81806926056963292, 37.62187500034138310, -42.41743335407646498 ) ) ;
#5117 = EDGE_CURVE ( 'NONE', #7989, #10461, #3893, .T. ) ;
#5118 = CARTESIAN_POINT ( 'NONE',  ( -49.99999999999999289, 29.88125000068279391, 16.24598481164533226 ) ) ;
#5119 = EDGE_CURVE ( 'NONE', #1042, #11555, #10663, .T. ) ;
#5120 = CARTESIAN_POINT ( 'NONE',  ( 49.99999999999999289, 29.10000000000000142, -16.24598481164532160 ) ) ;
#5121 = CARTESIAN_POINT ( 'NONE',  ( 9.631387414534489405E-15, 36.35937500034140157, 52.43083105670540789 ) ) ;
#5122 = CARTESIAN_POINT ( 'NONE',  ( -49.86468353125000164, 33.92187500034139447, 0.000000000000000000 ) ) ;
#5123 = EDGE_CURVE ( 'NONE', #12892, #4175, #2334, .T. ) ;
#5124 = CARTESIAN_POINT ( 'NONE',  ( -15.45084971874737256, 45.60000000000000142, -47.55282581475767500 ) ) ;
#5125 = ORIENTED_EDGE ( 'NONE', *, *, #7557, .T. ) ;
#5127 = VERTEX_POINT ( 'NONE', #9410 ) ;
#5126 =( BOUNDED_CURVE ( )  B_SPLINE_CURVE ( 2, ( #4892, #4981, #13595, #3551, #14920, #7381, #16258, #15093, #3720, #6056, #2202, #16012, #10947 ),
 .UNSPECIFIED., .F., .F. ) 
 B_SPLINE_CURVE_WITH_KNOTS ( ( 3, 2, 2, 2, 2, 2, 3 ),
 ( 0.5833333333333333703, 0.5866666666666666696, 0.5933333333333333792, 0.5999999999999999778, 0.6066666666666666874, 0.6133333333333332860, 0.6166666666666666963 ),
 .UNSPECIFIED. ) 
 CURVE ( )  GEOMETRIC_REPRESENTATION_ITEM ( )  RATIONAL_B_SPLINE_CURVE ( ( 0.9755282581475768211, 0.9755282581475771542, 1.000000000000000000, 0.9510565162951535312, 1.000000000000000000, 0.9510565162951535312, 1.000000000000000000, 0.9510565162951535312, 1.000000000000000000, 0.9510565162951535312, 1.000000000000000000, 0.9755282581475763770, 0.9755282581475768211 ) ) 
 REPRESENTATION_ITEM ( '' )  );
#5128 = CARTESIAN_POINT ( 'NONE',  ( 15.40903463028481113, 35.25937500034139305, -47.42413220539094709 ) ) ;
#5129 = ORIENTED_EDGE ( 'NONE', *, *, #6117, .F. ) ;
#5130 = ORIENTED_EDGE ( 'NONE', *, *, #11795, .F. ) ;
#5131 = CARTESIAN_POINT ( 'NONE',  ( 28.70358715772643166, 282.1599167565164521, -9.907174315453913138 ) ) ;
#5132 = CARTESIAN_POINT ( 'NONE',  ( -3.210462471511496205E-15, 47.35937500034138736, -52.43083105670540789 ) ) ;
#5133 = FACE_OUTER_BOUND ( 'NONE', #9934, .T. ) ;
#5134 = CARTESIAN_POINT ( 'NONE',  ( 49.86468353125000164, 26.92187500034139802, -6.106662507704105588E-15 ) ) ;
#5135 = DIRECTION ( 'NONE',  ( 0.000000000000000000, 0.000000000000000000, 1.000000000000000000 ) ) ;
#5136 = CARTESIAN_POINT ( 'NONE',  ( 9.631387414534489405E-15, 44.42187500034140157, 52.43083105670540789 ) ) ;
#5137 = CARTESIAN_POINT ( 'NONE',  ( 38.60409515610501074, 25.00000000000000000, -31.77615201968907144 ) ) ;
#5138 = CARTESIAN_POINT ( 'NONE',  ( 40.45084971874737079, 49.20000000000000284, -29.38926261462366440 ) ) ;
#5139 = CARTESIAN_POINT ( 'NONE',  ( 30.90169943749475578, 26.48125000068279888, 42.53254041760200010 ) ) ;
#5140 = CARTESIAN_POINT ( 'NONE',  ( -49.86468353125000164, 49.92187500034140157, 0.000000000000000000 ) ) ;
#5141 = CARTESIAN_POINT ( 'NONE',  ( 15.40903463028481113, 31.32187500034139305, -47.42413220539094709 ) ) ;
#5142 = CARTESIAN_POINT ( 'NONE',  ( 17.34476375915451740, 20.17423772944865945, 101.0000000000000000 ) ) ;
#5143 = ORIENTED_EDGE ( 'NONE', *, *, #4081, .F. ) ;
#5144 = VECTOR ( 'NONE', #10660, 1000.000000000000114 ) ;
#5145 = ORIENTED_EDGE ( 'NONE', *, *, #3249, .T. ) ;
#5146 = CARTESIAN_POINT ( 'NONE',  ( -2.547328955960238000E-13, 32.50000000000000000, 49.99999999999999289 ) ) ;
#5147 = LINE ( 'NONE', #6466, #16335 ) ;
#5148 = CARTESIAN_POINT ( 'NONE',  ( -30.90169943749474513, 23.69999999999999929, -42.53254041760200721 ) ) ;
#5149 = CARTESIAN_POINT ( 'NONE',  ( -7.500000000000000000, 25.00000000000000355, 39.29058411375428506 ) ) ;
#5150 = CARTESIAN_POINT ( 'NONE',  ( 49.86468353125000164, 32.85937500034139447, -6.106662507704105588E-15 ) ) ;
#5151 = CARTESIAN_POINT ( 'NONE',  ( 6.123233995736766085E-15, 20.00000000000000355, -50.00000000000000000 ) ) ;
#5152 = CARTESIAN_POINT ( 'NONE',  ( -49.86468353125000164, 47.92187500034139447, 0.000000000000000000 ) ) ;
#5153 = FACE_OUTER_BOUND ( 'NONE', #6481, .T. ) ;
#5154 = AXIS2_PLACEMENT_3D ( 'NONE', #2929, #7996, #338 ) ;
#5155 = CARTESIAN_POINT ( 'NONE',  ( -7.919222016226870942, 36.22999571913594963, 49.99999999999997158 ) ) ;
#5156 = DIRECTION ( 'NONE',  ( -0.000000000000000000, -0.000000000000000000, -1.000000000000000000 ) ) ;
#5157 = EDGE_LOOP ( 'NONE', ( #8102, #10104, #5992, #5888 ) ) ;
#5158 = CARTESIAN_POINT ( 'NONE',  ( -49.86468353124999453, 23.95937500034138878, 16.20201782572377525 ) ) ;
#5159 = EDGE_CURVE ( 'NONE', #14171, #7383, #6605, .T. ) ;
#5160 = ORIENTED_EDGE ( 'NONE', *, *, #3960, .F. ) ;
#5161 = CARTESIAN_POINT ( 'NONE',  ( -50.00000000000000000, 45.78125000068279604, 0.000000000000000000 ) ) ;
#5162 = VERTEX_POINT ( 'NONE', #5361 ) ;
#5163 = ORIENTED_EDGE ( 'NONE', *, *, #3030, .T. ) ;
#5164 = CYLINDRICAL_SURFACE ( 'NONE', #15546, 50.00000000000000000 ) ;
#5165 = CARTESIAN_POINT ( 'NONE',  ( 47.28673853953970507, 260.3313524089090265, -10.00000000000000178 ) ) ;
#5166 = CONICAL_SURFACE ( 'NONE', #5688, 16.50000000000000711, 0.7853981633974447263 ) ;
#5167 = DIRECTION ( 'NONE',  ( 0.000000000000000000, 0.000000000000000000, 1.000000000000000000 ) ) ;
#5168 = DIRECTION ( 'NONE',  ( -0.000000000000000000, -1.000000000000000000, -0.000000000000000000 ) ) ;
#5169 = CARTESIAN_POINT ( 'NONE',  ( 15.45084971874737789, 32.38125000068280457, 47.55282581475767500 ) ) ;
#5170 = LINE ( 'NONE', #10144, #16356 ) ;
#5171 = CARTESIAN_POINT ( 'NONE',  ( 0.000000000000000000, 280.0000000000000000, 0.000000000000000000 ) ) ;
#5172 = CARTESIAN_POINT ( 'NONE',  ( 0.000000000000000000, 217.0000000000000284, 0.000000000000000000 ) ) ;
#5173 = FILL_AREA_STYLE_COLOUR ( '', #9709 ) ;
#5174 = CARTESIAN_POINT ( 'NONE',  ( 1.022488062601840571E-14, 49.50000000000000711, -50.00000000000000000 ) ) ;
#5175 = CARTESIAN_POINT ( 'NONE',  ( 40.45084971874737079, 40.98125000068279888, -29.38926261462366440 ) ) ;
#5176 = CARTESIAN_POINT ( 'NONE',  ( 2.600676159226420495E-13, 21.50000000000000000, -49.99999999999999289 ) ) ;
#5177 = CARTESIAN_POINT ( 'NONE',  ( 50.00000000000000711, 20.90000000000000213, 16.24598481164530739 ) ) ;
#5178 = SURFACE_STYLE_USAGE ( .BOTH. , #7737 ) ;
#5179 = ORIENTED_EDGE ( 'NONE', *, *, #283, .T. ) ;
#5180 = VECTOR ( 'NONE', #13031, 1000.000000000000000 ) ;
#5181 = CARTESIAN_POINT ( 'NONE',  ( -15.40903463028481646, 45.45937500034139589, -47.42413220539093999 ) ) ;
#5182 = EDGE_LOOP ( 'NONE', ( #14496, #10965, #8865, #15210 ) ) ;
#5183 = LINE ( 'NONE', #8993, #386 ) ;
#5184 = FACE_OUTER_BOUND ( 'NONE', #14025, .T. ) ;
#5185 = CARTESIAN_POINT ( 'NONE',  ( -30.81806926056962226, 30.15937500034139163, 42.41743335407647919 ) ) ;
#5186 = ORIENTED_EDGE ( 'NONE', *, *, #9680, .F. ) ;
#5187 = CARTESIAN_POINT ( 'NONE',  ( 30.90169943749473802, 27.29999999999999716, -42.53254041760200721 ) ) ;
#5188 = CARTESIAN_POINT ( 'NONE',  ( 19.99999999999999289, 312.0000000000000568, -2.499999999999999556 ) ) ;
#5189 = VECTOR ( 'NONE', #8202, 1000.000000000000000 ) ;
#5190 = CARTESIAN_POINT ( 'NONE',  ( 6.123233995736766085E-15, 52.00000000000000711, 50.00000000000000000 ) ) ;
#5191 = CARTESIAN_POINT ( 'NONE',  ( -49.86468353124999453, 34.02187500034140299, 16.20201782572377169 ) ) ;
#5192 = AXIS2_PLACEMENT_3D ( 'NONE', #3323, #14950, #3239 ) ;
#5193 = CARTESIAN_POINT ( 'NONE',  ( -3.210462471511496205E-15, 23.35937500034139447, -52.43083105670540789 ) ) ;
#5194 = DIRECTION ( 'NONE',  ( 0.000000000000000000, 1.000000000000000000, 0.000000000000000000 ) ) ;
#5195 = CARTESIAN_POINT ( 'NONE',  ( 49.86468353124999453, 27.02187500034139944, -16.20201782572376104 ) ) ;
#5196 = CARTESIAN_POINT ( 'NONE',  ( -30.90169943749474513, 29.48125000068279888, -42.53254041760200721 ) ) ;
#5197 = CARTESIAN_POINT ( 'NONE',  ( -50.00000000000000000, 32.00000000000000000, 0.000000000000000000 ) ) ;
#5198 = CARTESIAN_POINT ( 'NONE',  ( -49.86468353124999453, 35.75937500034140015, -16.20201782572375393 ) ) ;
#5199 = CARTESIAN_POINT ( 'NONE',  ( 15.40903463028482356, 34.52187500034140299, 47.42413220539093999 ) ) ;
#5200 = EDGE_CURVE ( 'NONE', #11991, #14378, #4969, .T. ) ;
#5201 = CARTESIAN_POINT ( 'NONE',  ( 50.00000000000000000, 41.00000000000000000, -6.123233995736766085E-15 ) ) ;
#5202 = ORIENTED_EDGE ( 'NONE', *, *, #12196, .T. ) ;
#5203 = AXIS2_PLACEMENT_3D ( 'NONE', #7541, #3885, #15255 ) ;
#5204 = CARTESIAN_POINT ( 'NONE',  ( 40.34137639590981905, 34.65937500034139873, 29.30972558990010768 ) ) ;
#5205 = ORIENTED_EDGE ( 'NONE', *, *, #9291, .T. ) ;
#5206 = ORIENTED_EDGE ( 'NONE', *, *, #8853, .F. ) ;
#5207 = EDGE_CURVE ( 'NONE', #16078, #10616, #14229, .T. ) ;
#5208 = CARTESIAN_POINT ( 'NONE',  ( 28.69101924422354699, 282.0322304394513253, -11.84550962211230107 ) ) ;
#5210 = ADVANCED_FACE ( 'NONE', ( #4186 ), #2928, .T. ) ;
#5209 = CARTESIAN_POINT ( 'NONE',  ( 30.90169943749474157, 21.08125000068279675, -42.53254041760200721 ) ) ;
#5211 = CARTESIAN_POINT ( 'NONE',  ( -3.589930709342005422, 98.09116937221706678, -5.000000000000000000 ) ) ;
#5212 = CARTESIAN_POINT ( 'NONE',  ( 15.40903463028481113, 23.32187500034139660, -47.42413220539094709 ) ) ;
#5213 = CARTESIAN_POINT ( 'NONE',  ( -25.00000000000000711, 284.0710678118654755, 2.500000000000003109 ) ) ;
#5214 = EDGE_CURVE ( 'NONE', #2087, #12474, #6854, .T. ) ;
#5215 = CARTESIAN_POINT ( 'NONE',  ( -15.40903463028481646, 43.52187500034139589, -47.42413220539093999 ) ) ;
#5216 = CARTESIAN_POINT ( 'NONE',  ( -30.81806926056963292, 39.55937500034140442, -42.41743335407646498 ) ) ;
#5217 = CARTESIAN_POINT ( 'NONE',  ( 2.500000000000000000, 242.0000000000000284, 40.00000000000000000 ) ) ;
#5218 = AXIS2_PLACEMENT_3D ( 'NONE', #15750, #14342, #13023 ) ;
#5219 = CARTESIAN_POINT ( 'NONE',  ( 30.90169943749475578, 44.69999999999999574, 42.53254041760200010 ) ) ;
#5220 = PRODUCT ( 'Speed Control Knob & Dial', 'Speed Control Knob & Dial', '', ( #13346 ) ) ;
#5221 = CARTESIAN_POINT ( 'NONE',  ( -50.00000000000000000, 27.78125000068279959, 0.000000000000000000 ) ) ;
#5222 = CARTESIAN_POINT ( 'NONE',  ( 40.34137639590981195, 49.12187500034139731, -29.30972558990011834 ) ) ;
#5223 =( BOUNDED_CURVE ( )  B_SPLINE_CURVE ( 3, ( #13453, #12036, #1968, #9557 ),
 .UNSPECIFIED., .F., .T. ) 
 B_SPLINE_CURVE_WITH_KNOTS ( ( 4, 4 ),
 ( 1.570796326794896780, 3.141592653589793116 ),
 .UNSPECIFIED. ) 
 CURVE ( )  GEOMETRIC_REPRESENTATION_ITEM ( )  RATIONAL_B_SPLINE_CURVE ( ( 1.000000000000000000, 0.8047378541243650485, 0.8047378541243650485, 1.000000000000000000 ) ) 
 REPRESENTATION_ITEM ( '' )  );
#5224 = EDGE_CURVE ( 'NONE', #3644, #7740, #7248, .T. ) ;
#5225 = CARTESIAN_POINT ( 'NONE',  ( 49.86468353124999453, 33.02187500034139589, -16.20201782572376459 ) ) ;
#5226 = PLANE ( 'NONE',  #3836 ) ;
#5227 = CLOSED_SHELL ( 'NONE', ( #3399, #12072, #1534, #7840, #14756, #1079 ) ) ;
#5228 = EDGE_LOOP ( 'NONE', ( #799, #9813, #2199, #4662 ) ) ;
#5229 = AXIS2_PLACEMENT_3D ( 'NONE', #1444, #10350, #7692 ) ;
#5230 = AXIS2_PLACEMENT_3D ( 'NONE', #5469, #15598, #9286 ) ;
#5231 = AXIS2_PLACEMENT_3D ( 'NONE', #3328, #2076, #828 ) ;
#5232 = EDGE_LOOP ( 'NONE', ( #12679, #15207, #10306, #12693 ) ) ;
#5233 =( GEOMETRIC_REPRESENTATION_CONTEXT ( 3 ) GLOBAL_UNCERTAINTY_ASSIGNED_CONTEXT ( ( #15231 ) ) GLOBAL_UNIT_ASSIGNED_CONTEXT ( ( #14936, #15104, #13933 ) ) REPRESENTATION_CONTEXT ( 'NONE', 'WORKASPACE' ) );
#5234 = CARTESIAN_POINT ( 'NONE',  ( -49.99999999999999289, 31.89999999999999858, -16.24598481164531449 ) ) ;
#5235 = CARTESIAN_POINT ( 'NONE',  ( 15.45084971874736723, 45.40000000000000568, -47.55282581475768211 ) ) ;
#5236 = EDGE_CURVE ( 'NONE', #6058, #1228, #5837, .T. ) ;
#5237 = DIRECTION ( 'NONE',  ( -0.000000000000000000, 1.000000000000000000, -0.000000000000000000 ) ) ;
#5238 = CARTESIAN_POINT ( 'NONE',  ( -40.34137639590981195, 46.12187500034139731, 29.30972558990012189 ) ) ;
#5239 = CARTESIAN_POINT ( 'NONE',  ( -49.86468353125000164, 33.85937500034139447, 0.000000000000000000 ) ) ;
#5240 = CARTESIAN_POINT ( 'NONE',  ( 7.500000000000000000, 25.00000000000000355, 39.29058411375427795 ) ) ;
#5241 = CARTESIAN_POINT ( 'NONE',  ( -49.86468353124999453, 43.82187500034140015, -16.20201782572375393 ) ) ;
#5242 = VECTOR ( 'NONE', #15, 1000.000000000000000 ) ;
#5243 = AXIS2_PLACEMENT_3D ( 'NONE', #12325, #3523, #9844 ) ;
#5244 = LINE ( 'NONE', #15606, #2227 ) ;
#5246 = ADVANCED_FACE ( 'NONE', ( #13629 ), #2819, .T. ) ;
#5245 = AXIS2_PLACEMENT_3D ( 'NONE', #4604, #9664, #16309 ) ;
#5247 = CARTESIAN_POINT ( 'NONE',  ( 0.000000000000000000, 51.99999999999999289, 0.000000000000000000 ) ) ;
#5248 = CARTESIAN_POINT ( 'NONE',  ( 0.1743114854953164983, 100.0076106038165165, -5.000000000000000000 ) ) ;
#5249 = VERTEX_POINT ( 'NONE', #15966 ) ;
#5250 = CARTESIAN_POINT ( 'NONE',  ( -49.86468353125000164, 19.85937500034139447, 0.000000000000000000 ) ) ;
#5251 = VERTEX_POINT ( 'NONE', #12229 ) ;
#5252 = CARTESIAN_POINT ( 'NONE',  ( 7.394441145214595501, 28.48516834767053751, 101.0000000000000000 ) ) ;
#5253 = EDGE_LOOP ( 'NONE', ( #39, #14838, #139, #10062 ) ) ;
#5254 = ORIENTED_EDGE ( 'NONE', *, *, #13416, .F. ) ;
#5255 = CIRCLE ( 'NONE', #11607, 17.50000000000000000 ) ;
#5256 = EDGE_CURVE ( 'NONE', #7399, #4332, #11327, .T. ) ;
#5257 = CARTESIAN_POINT ( 'NONE',  ( 0.000000000000000000, 22.50000000000000000, 102.0000000000000142 ) ) ;
#5258 = CARTESIAN_POINT ( 'NONE',  ( -9.877534094663211306, 8.054089844915763408, 101.0000000000000000 ) ) ;
#5259 = DIRECTION ( 'NONE',  ( 0.000000000000000000, 0.000000000000000000, -1.000000000000000000 ) ) ;
#5260 = CARTESIAN_POINT ( 'NONE',  ( 12.67046914267482016, 34.58135802401886139, 102.0000000000000142 ) ) ;
#5261 = DIRECTION ( 'NONE',  ( -0.9945218953682744001, 0.1045284632676435066, 0.000000000000000000 ) ) ;
#5262 = CARTESIAN_POINT ( 'NONE',  ( -1.572311786628345809, 98.28009660169102801, 5.000000000000000000 ) ) ;
#5263 = CARTESIAN_POINT ( 'NONE',  ( -6.668400408272873429E-15, 49.28125000068279604, -50.00000000000000000 ) ) ;
#5264 = FACE_OUTER_BOUND ( 'NONE', #9375, .T. ) ;
#5265 = CYLINDRICAL_SURFACE ( 'NONE', #10991, 50.00000000000000000 ) ;
#5266 = CARTESIAN_POINT ( 'NONE',  ( 15.45084971874737789, 38.38125000068279746, 47.55282581475767500 ) ) ;
#5267 = CARTESIAN_POINT ( 'NONE',  ( 0.000000000000000000, 20.00000000000000355, 50.00000000000000000 ) ) ;
#5268 = CARTESIAN_POINT ( 'NONE',  ( 49.99999999999999289, 25.10000000000000142, -16.24598481164532160 ) ) ;
#5269 = CARTESIAN_POINT ( 'NONE',  ( -17.45639740057859868, 21.16801284050013976, 101.0000000000000000 ) ) ;
#5270 = ORIENTED_EDGE ( 'NONE', *, *, #8290, .F. ) ;
#5271 = CARTESIAN_POINT ( 'NONE',  ( 49.86468353125001585, 36.75937500034138594, 16.20201782572375038 ) ) ;
#5272 = ORIENTED_EDGE ( 'NONE', *, *, #4314, .F. ) ;
#5273 = CARTESIAN_POINT ( 'NONE',  ( 50.00000000000000000, 42.78125000068280315, -6.123233995736766085E-15 ) ) ;
#5274 = AXIS2_PLACEMENT_3D ( 'NONE', #4791, #14981, #8672 ) ;
#5275 = CARTESIAN_POINT ( 'NONE',  ( -25.00000000000000355, 287.0000000000000568, -2.499999999999998668 ) ) ;
#5276 = CARTESIAN_POINT ( 'NONE',  ( -15.40903463028481646, 31.45937500034139944, -47.42413220539093999 ) ) ;
#5277 = ORIENTED_EDGE ( 'NONE', *, *, #8180, .F. ) ;
#5278 = FACE_OUTER_BOUND ( 'NONE', #13417, .T. ) ;
#5279 = LINE ( 'NONE', #11566, #16085 ) ;
#5280 = CARTESIAN_POINT ( 'NONE',  ( 46.50201513659349217, 25.00000000000000000, -18.00136805656013905 ) ) ;
#5281 = CARTESIAN_POINT ( 'NONE',  ( -3.210462471511496205E-15, 31.42187500034139447, -52.43083105670540789 ) ) ;
#5282 = EDGE_CURVE ( 'NONE', #1352, #16058, #13069, .T. ) ;
#5283 = CARTESIAN_POINT ( 'NONE',  ( 30.81806926056964002, 22.55937500034139020, 42.41743335407646498 ) ) ;
#5284 = CARTESIAN_POINT ( 'NONE',  ( -3.505380114644273348, 100.5662537783983908, 8.566253778398339236 ) ) ;
#5285 = CARTESIAN_POINT ( 'NONE',  ( 30.81806926056964002, 28.62187500034139731, 42.41743335407646498 ) ) ;
#5286 = LINE ( 'NONE', #2680, #5242 ) ;
#5287 = CARTESIAN_POINT ( 'NONE',  ( 9.657523855033129090E-15, 28.49999999999999645, 52.57311121191334990 ) ) ;
#5288 = CARTESIAN_POINT ( 'NONE',  ( 9.631387414534489405E-15, 34.35937500034139447, 52.43083105670540789 ) ) ;
#5289 = CARTESIAN_POINT ( 'NONE',  ( 15.40903463028482356, 30.52187500034139589, 47.42413220539093999 ) ) ;
#5290 = AXIS2_PLACEMENT_3D ( 'NONE', #15024, #6475, #8712 ) ;
#5291 = VERTEX_POINT ( 'NONE', #7087 ) ;
#5292 = PRODUCT_DEFINITION_CONTEXT ( 'detailed design', #13231, 'design' ) ;
#5293 = CARTESIAN_POINT ( 'NONE',  ( -49.86468353125000164, 33.85937500034139447, 0.000000000000000000 ) ) ;
#5294 = EDGE_CURVE ( 'NONE', #12450, #16417, #2220, .T. ) ;
#5295 = ORIENTED_EDGE ( 'NONE', *, *, #10543, .T. ) ;
#5296 = ORIENTED_EDGE ( 'NONE', *, *, #14531, .F. ) ;
#5297 = CARTESIAN_POINT ( 'NONE',  ( 28.38892170791706704, 282.2553694771637538, -9.277843415834380991 ) ) ;
#5298 = CARTESIAN_POINT ( 'NONE',  ( -15.40903463028481646, 45.45937500034139589, -47.42413220539093999 ) ) ;
#5299 = PLANE ( 'NONE',  #4919 ) ;
#5300 = CARTESIAN_POINT ( 'NONE',  ( -15.40903463028480580, 24.32187500034139660, 47.42413220539094709 ) ) ;
#5301 = FACE_OUTER_BOUND ( 'NONE', #980, .T. ) ;
#5302 = CARTESIAN_POINT ( 'NONE',  ( -40.34137639590981195, 38.12187500034139731, 29.30972558990012189 ) ) ;
#5303 = CARTESIAN_POINT ( 'NONE',  ( -30.81806926056962226, 40.15937500034139163, 42.41743335407647209 ) ) ;
#5304 = CARTESIAN_POINT ( 'NONE',  ( -14.89925740754307881, 13.32055945583976353, 101.0000000000000000 ) ) ;
#5305 = CARTESIAN_POINT ( 'NONE',  ( -3.219174618344376363E-15, 45.49999999999999289, -52.57311121191334990 ) ) ;
#5306 = CARTESIAN_POINT ( 'NONE',  ( -49.99999999999999289, 21.68125000068280173, -16.24598481164531449 ) ) ;
#5307 = EDGE_CURVE ( 'NONE', #6137, #13242, #2964, .T. ) ;
#5308 = CARTESIAN_POINT ( 'NONE',  ( -40.34137639590981905, 49.72187500034139873, -29.30972558990011478 ) ) ;
#5309 = CARTESIAN_POINT ( 'NONE',  ( 15.40903463028482356, 26.52187500034139589, 47.42413220539093999 ) ) ;
#5310 = CARTESIAN_POINT ( 'NONE',  ( 8.446640517145639571E-15, 28.28125000068279959, 50.00000000000000000 ) ) ;
#5311 = ORIENTED_EDGE ( 'NONE', *, *, #210, .F. ) ;
#5312 = CARTESIAN_POINT ( 'NONE',  ( 15.45084971874736723, 39.18125000068280173, -47.55282581475768211 ) ) ;
#5313 = EDGE_LOOP ( 'NONE', ( #119, #2025, #14356, #4861, #13040 ) ) ;
#5314 = CARTESIAN_POINT ( 'NONE',  ( 0.000000000000000000, 22.50000000000000000, 100.0000000000000000 ) ) ;
#5315 = PLANE ( 'NONE',  #6815 ) ;
#5316 = EDGE_CURVE ( 'NONE', #4152, #9378, #2553, .T. ) ;
#5317 = DIRECTION ( 'NONE',  ( -0.03463303435789753804, 0.9463120918278141724, 0.3213938048432660732 ) ) ;
#5318 = CARTESIAN_POINT ( 'NONE',  ( 15.40903463028482356, 44.52187500034139589, 47.42413220539093999 ) ) ;
#5319 = CARTESIAN_POINT ( 'NONE',  ( 15.40903463028482356, 26.45937500034139589, 47.42413220539093999 ) ) ;
#5320 = DIRECTION ( 'NONE',  ( 0.000000000000000000, 0.7071067811865487940, -0.7071067811865463515 ) ) ;
#5321 = DIRECTION ( 'NONE',  ( 0.000000000000000000, 0.000000000000000000, -1.000000000000000000 ) ) ;
#5322 = CARTESIAN_POINT ( 'NONE',  ( -15.40903463028481646, 45.52187500034139589, -47.42413220539093999 ) ) ;
#5323 = ADVANCED_FACE ( 'NONE', ( #3424 ), #2157, .T. ) ;
#5324 = COLOUR_RGB ( '', 0.09019608, 0.27058824, 0.51372549) ;
#5325 = APPLICATION_PROTOCOL_DEFINITION ( 'draft international standard', 'automotive_design', 1998, #12159 ) ;
#5326 = CYLINDRICAL_SURFACE ( 'NONE', #1441, 50.00000000000000000 ) ;
#5327 = CARTESIAN_POINT ( 'NONE',  ( 30.81806926056962936, 47.22187500034139873, -42.41743335407647209 ) ) ;
#5328 = DIRECTION ( 'NONE',  ( 0.9993309688977880523, 0.03657341386592528887, -0.000000000000000000 ) ) ;
#5329 = ORIENTED_EDGE ( 'NONE', *, *, #5224, .F. ) ;
#5330 = EDGE_CURVE ( 'NONE', #3621, #15902, #12950, .T. ) ;
#5331 = CARTESIAN_POINT ( 'NONE',  ( -49.86468353124999453, 45.82187500034140015, -16.20201782572375393 ) ) ;
#5332 = ORIENTED_EDGE ( 'NONE', *, *, #29, .F. ) ;
#5333 = DIRECTION ( 'NONE',  ( 0.000000000000000000, 0.000000000000000000, 1.000000000000000000 ) ) ;
#5334 = ORIENTED_EDGE ( 'NONE', *, *, #8123, .T. ) ;
#5335 = VERTEX_POINT ( 'NONE', #8809 ) ;
#5336 = DIRECTION ( 'NONE',  ( -1.000000000000000000, 0.000000000000000000, 0.000000000000000000 ) ) ;
#5337 = DIRECTION ( 'NONE',  ( 0.000000000000000000, 0.000000000000000000, 1.000000000000000000 ) ) ;
#5338 = CARTESIAN_POINT ( 'NONE',  ( -49.99999999999999289, 27.89999999999999858, -16.24598481164531449 ) ) ;
#5339 = CARTESIAN_POINT ( 'NONE',  ( -30.90169943749474868, 21.69999999999999574, -42.53254041760200721 ) ) ;
#5340 = CARTESIAN_POINT ( 'NONE',  ( -15.40903463028481646, 49.45937500034140299, -47.42413220539093999 ) ) ;
#5341 = CARTESIAN_POINT ( 'NONE',  ( -40.45084971874737079, 31.98125000068280244, 29.38926261462367151 ) ) ;
#5342 = DIRECTION ( 'NONE',  ( -2.312964634635742464E-16, 0.000000000000000000, -1.000000000000000000 ) ) ;
#5343 = CARTESIAN_POINT ( 'NONE',  ( -30.81806926056962226, 24.22187500034139163, 42.41743335407647919 ) ) ;
#5344 = DIRECTION ( 'NONE',  ( -0.000000000000000000, -0.000000000000000000, 1.000000000000000000 ) ) ;
#5345 = CARTESIAN_POINT ( 'NONE',  ( 30.90169943749475578, 42.48125000068279888, 42.53254041760200010 ) ) ;
#5346 = CARTESIAN_POINT ( 'NONE',  ( 0.000000000000000000, 22.50000000000000000, 101.0000000000000000 ) ) ;
#5347 = CARTESIAN_POINT ( 'NONE',  ( 30.90169943749474157, 23.29999999999999716, -42.53254041760200721 ) ) ;
#5348 = ADVANCED_FACE ( 'NONE', ( #2488 ), #16369, .T. ) ;
#5349 = ORIENTED_EDGE ( 'NONE', *, *, #6117, .T. ) ;
#5350 = CARTESIAN_POINT ( 'NONE',  ( -49.86468353124999453, 39.75937500034139305, -16.20201782572375393 ) ) ;
#5351 = ORIENTED_EDGE ( 'NONE', *, *, #5159, .F. ) ;
#5352 = CARTESIAN_POINT ( 'NONE',  ( 30.90169943749475223, 42.69999999999999574, 42.53254041760199300 ) ) ;
#5353 = DIRECTION ( 'NONE',  ( 1.156482317317871478E-16, 0.000000000000000000, 1.000000000000000000 ) ) ;
#5354 = CARTESIAN_POINT ( 'NONE',  ( 9.631387414534489405E-15, 28.35937500034139802, 52.43083105670540789 ) ) ;
#5355 = VERTEX_POINT ( 'NONE', #10070 ) ;
#5356 = B_SPLINE_CURVE_WITH_KNOTS ( 'NONE', 3,
 ( #12713, #16285, #1482, #7724 ),
 .UNSPECIFIED., .F., .F.,
 ( 4, 4 ),
 ( 2.829004760659353259E-07, 0.001414802801989363968 ),
 .UNSPECIFIED. ) ;
#5357 = CARTESIAN_POINT ( 'NONE',  ( 0.000000000000000000, 267.0000000000000000, 0.000000000000000000 ) ) ;
#5358 = DIRECTION ( 'NONE',  ( 0.000000000000000000, 0.000000000000000000, -1.000000000000000000 ) ) ;
#5359 = PLANE ( 'NONE',  #600 ) ;
#5360 = CARTESIAN_POINT ( 'NONE',  ( 40.34137639590981195, 35.12187500034139731, -29.30972558990011834 ) ) ;
#5361 = CARTESIAN_POINT ( 'NONE',  ( 0.000000000000000000, 51.99999999999999289, -47.00000000000000000 ) ) ;
#5362 = LINE ( 'NONE', #11905, #5678 ) ;
#5363 = CARTESIAN_POINT ( 'NONE',  ( -46.91068958262638944, 20.00000000000000355, 16.90862634959490407 ) ) ;
#5364 = CARTESIAN_POINT ( 'NONE',  ( 49.86468353125001585, 26.82187500034139305, 16.20201782572375038 ) ) ;
#5365 = PLANE ( 'NONE',  #9224 ) ;
#5366 = CARTESIAN_POINT ( 'NONE',  ( -49.99999999999999289, 32.10000000000000142, 16.24598481164533226 ) ) ;
#5367 = CARTESIAN_POINT ( 'NONE',  ( -40.34137639590981195, 34.05937500034139731, 29.30972558990012189 ) ) ;
#5368 = CARTESIAN_POINT ( 'NONE',  ( -49.86468353124999453, 27.82187500034139305, -16.20201782572375393 ) ) ;
#5369 = DIRECTION ( 'NONE',  ( -0.000000000000000000, 1.000000000000000000, -0.000000000000000000 ) ) ;
#5370 = ORIENTED_EDGE ( 'NONE', *, *, #4856, .T. ) ;
#5371 = EDGE_CURVE ( 'NONE', #11650, #8003, #6093, .T. ) ;
#5372 = CARTESIAN_POINT ( 'NONE',  ( 49.86468353124999453, 36.95937500034139589, -16.20201782572376104 ) ) ;
#5373 = ADVANCED_FACE ( 'NONE', ( #11238 ), #16216, .T. ) ;
#5374 = VERTEX_POINT ( 'NONE', #2797 ) ;
#5375 = CARTESIAN_POINT ( 'NONE',  ( 27.61612561545959821, 282.5087415087664340, -10.11612561546112943 ) ) ;
#5376 = CARTESIAN_POINT ( 'NONE',  ( -49.99999999999999289, 19.88125000068279746, 16.24598481164533226 ) ) ;
#5377 = DIRECTION ( 'NONE',  ( -0.8660254037844320463, 0.5000000000000113243, 0.000000000000000000 ) ) ;
#5378 = CARTESIAN_POINT ( 'NONE',  ( -26.02446187185519832, 283.9500510409137632, 4.548923743721434043 ) ) ;
#5379 = CARTESIAN_POINT ( 'NONE',  ( -49.86468353124999453, 33.82187500034138594, -16.20201782572375393 ) ) ;
#5380 = CARTESIAN_POINT ( 'NONE',  ( -49.86468353124999453, 43.75937500034140015, -16.20201782572375393 ) ) ;
#5381 = CARTESIAN_POINT ( 'NONE',  ( 1.490838860747792127E-14, 52.00000000000002132, 44.99999999999998579 ) ) ;
#5382 = CARTESIAN_POINT ( 'NONE',  ( -15.45084971874736368, 44.39999999999999858, 47.55282581475768211 ) ) ;
#5383 = CARTESIAN_POINT ( 'NONE',  ( -15.45084971874736368, 22.18125000068279817, 47.55282581475768211 ) ) ;
#5384 = CARTESIAN_POINT ( 'NONE',  ( 40.34137639590981195, 29.12187500034139376, -29.30972558990011834 ) ) ;
#5385 = ORIENTED_EDGE ( 'NONE', *, *, #16286, .F. ) ;
#5386 = CARTESIAN_POINT ( 'NONE',  ( -3.219174618344376363E-15, 37.28125000068280315, -52.57311121191334990 ) ) ;
#5387 = VERTEX_POINT ( 'NONE', #7871 ) ;
#5388 = DIRECTION ( 'NONE',  ( -1.000000000000000000, 0.000000000000000000, -2.312964634635742464E-16 ) ) ;
#5389 = CARTESIAN_POINT ( 'NONE',  ( 9.220054415934899174E-15, 45.00000000000001421, -2.129832066681984848E-14 ) ) ;
#5390 = CARTESIAN_POINT ( 'NONE',  ( 1.037474003217658816E-14, 102.0000000000000142, 9.080892972013893782 ) ) ;
#5391 = CARTESIAN_POINT ( 'NONE',  ( -30.81806926056962226, 46.22187500034139163, 42.41743335407647209 ) ) ;
#5392 = CARTESIAN_POINT ( 'NONE',  ( -15.40903463028480580, 22.25937500034139660, 47.42413220539094709 ) ) ;
#5393 = DIRECTION ( 'NONE',  ( -0.000000000000000000, -1.000000000000000000, -0.000000000000000000 ) ) ;
#5394 = CARTESIAN_POINT ( 'NONE',  ( -30.81806926056962226, 40.22187500034139873, 42.41743335407647209 ) ) ;
#5395 = PRODUCT_CONTEXT ( 'NONE', #10998, 'mechanical' ) ;
#5396 = CARTESIAN_POINT ( 'NONE',  ( 49.95625437244530787, 25.00000000000000000, -4.103175251694326953 ) ) ;
#5397 = CARTESIAN_POINT ( 'NONE',  ( 40.34137639590981195, 47.12187500034140442, -29.30972558990011834 ) ) ;
#5398 = CARTESIAN_POINT ( 'NONE',  ( 49.99999999999999289, 28.88125000068279391, -16.24598481164532160 ) ) ;
#5399 = ORIENTED_EDGE ( 'NONE', *, *, #14670, .F. ) ;
#5400 = EDGE_CURVE ( 'NONE', #7011, #13460, #16112, .T. ) ;
#5401 = AXIS2_PLACEMENT_3D ( 'NONE', #3313, #4495, #13370 ) ;
#5402 = CARTESIAN_POINT ( 'NONE',  ( -15.40903463028481646, 49.52187500034140299, -47.42413220539093999 ) ) ;
#5403 = ORIENTED_EDGE ( 'NONE', *, *, #3603, .T. ) ;
#5404 = CARTESIAN_POINT ( 'NONE',  ( -15.45084971874737256, 25.60000000000000142, -47.55282581475767500 ) ) ;
#5405 = ORIENTED_EDGE ( 'NONE', *, *, #1271, .F. ) ;
#5406 = ORIENTED_EDGE ( 'NONE', *, *, #9936, .T. ) ;
#5407 = CARTESIAN_POINT ( 'NONE',  ( -3.111920190527341144E-15, 43.28125000068280315, -50.00000000000000000 ) ) ;
#5408 = CARTESIAN_POINT ( 'NONE',  ( 15.45084971874736723, 39.18125000068280173, -47.55282581475768211 ) ) ;
#5410 = EDGE_CURVE ( 'NONE', #7762, #15191, #9905, .T. ) ;
#5409 =( BOUNDED_CURVE ( )  B_SPLINE_CURVE ( 3, ( #11511, #2444, #5213, #12762 ),
 .UNSPECIFIED., .F., .T. ) 
 B_SPLINE_CURVE_WITH_KNOTS ( ( 4, 4 ),
 ( 1.570796326794896780, 3.141592653589793116 ),
 .UNSPECIFIED. ) 
 CURVE ( )  GEOMETRIC_REPRESENTATION_ITEM ( )  RATIONAL_B_SPLINE_CURVE ( ( 1.000000000000000000, 0.8047378541243650485, 0.8047378541243650485, 1.000000000000000000 ) ) 
 REPRESENTATION_ITEM ( '' )  );
#5411 = CARTESIAN_POINT ( 'NONE',  ( -15.45084971874737256, 27.60000000000000142, -47.55282581475767500 ) ) ;
#5412 = CARTESIAN_POINT ( 'NONE',  ( -15.40903463028480580, 42.25937500034139305, 47.42413220539094709 ) ) ;
#5413 = CARTESIAN_POINT ( 'NONE',  ( -2.500000000000000000, 245.0000000000000284, 49.99999999999999289 ) ) ;
#5414 = AXIS2_PLACEMENT_3D ( 'NONE', #7993, #13144, #15554 ) ;
#5415 = CARTESIAN_POINT ( 'NONE',  ( -30.81806926056963292, 21.62187500034139376, -42.41743335407647209 ) ) ;
#5416 = EDGE_CURVE ( 'NONE', #11934, #2664, #7412, .T. ) ;
#5417 = DIRECTION ( 'NONE',  ( 0.000000000000000000, 1.000000000000000000, 0.000000000000000000 ) ) ;
#5418 = CARTESIAN_POINT ( 'NONE',  ( -30.90169943749474868, 41.48125000068278467, -42.53254041760200721 ) ) ;
#5419 = FACE_OUTER_BOUND ( 'NONE', #10691, .T. ) ;
#5420 = DIRECTION ( 'NONE',  ( 0.000000000000000000, 1.000000000000000000, -0.000000000000000000 ) ) ;
#5421 = DIRECTION ( 'NONE',  ( 0.000000000000000000, 0.000000000000000000, -1.000000000000000000 ) ) ;
#5422 = ORIENTED_EDGE ( 'NONE', *, *, #10862, .F. ) ;
#5423 = ADVANCED_FACE ( 'NONE', ( #9987 ), #1240, .T. ) ;
#5424 = CARTESIAN_POINT ( 'NONE',  ( -15.40903463028480580, 36.25937500034140015, 47.42413220539094709 ) ) ;
#5425 = ORIENTED_EDGE ( 'NONE', *, *, #15590, .T. ) ;
#5426 = EDGE_LOOP ( 'NONE', ( #13925, #3661, #2360, #9220 ) ) ;
#5427 = AXIS2_PLACEMENT_3D ( 'NONE', #3582, #2575, #11396 ) ;
#5428 = CARTESIAN_POINT ( 'NONE',  ( 9.657523855033129090E-15, 48.28125000068279604, 52.57311121191334990 ) ) ;
#5429 = PLANE ( 'NONE',  #1233 ) ;
#5430 = CARTESIAN_POINT ( 'NONE',  ( -49.86468353124999453, 21.95937500034138878, 16.20201782572377525 ) ) ;
#5431 = EDGE_LOOP ( 'NONE', ( #9971, #3138, #7314, #7575 ) ) ;
#5432 = CARTESIAN_POINT ( 'NONE',  ( -15.45084971874736368, 48.40000000000000568, 47.55282581475768211 ) ) ;
#5433 = PLANE ( 'NONE',  #3080 ) ;
#5434 = DIRECTION ( 'NONE',  ( 0.000000000000000000, 0.000000000000000000, 1.000000000000000000 ) ) ;
#5435 = CARTESIAN_POINT ( 'NONE',  ( 40.34137639590981905, 26.72187500034139518, 29.30972558990010768 ) ) ;
#5436 = CARTESIAN_POINT ( 'NONE',  ( 9.366734789577542680E-15, 82.00000000000001421, -2.024759949320127682E-14 ) ) ;
#5437 = DIRECTION ( 'NONE',  ( -0.4999999999999977796, 0.000000000000000000, 0.8660254037844399289 ) ) ;
#5438 = CARTESIAN_POINT ( 'NONE',  ( -47.60088917010773457, 20.00000000000000355, 14.85495851097764231 ) ) ;
#5439 = CARTESIAN_POINT ( 'NONE',  ( -49.86468353124999453, 26.02187500034139589, 16.20201782572377169 ) ) ;
#5440 = CYLINDRICAL_SURFACE ( 'NONE', #3094, 5.000000000000000000 ) ;
#5441 = VECTOR ( 'NONE', #9476, 999.9999999999998863 ) ;
#5442 = CARTESIAN_POINT ( 'NONE',  ( 40.45084971874737079, 35.20000000000000284, -29.38926261462366440 ) ) ;
#5443 = CARTESIAN_POINT ( 'NONE',  ( 40.34137639590981195, 31.05937500034139731, -29.30972558990011834 ) ) ;
#5444 = ADVANCED_FACE ( 'NONE', ( #992 ), #9210, .T. ) ;
#5445 = LINE ( 'NONE', #13241, #6201 ) ;
#5446 = ORIENTED_EDGE ( 'NONE', *, *, #12365, .T. ) ;
#5447 = CARTESIAN_POINT ( 'NONE',  ( 49.86468353125000164, 26.85937500034139802, -6.106662507704105588E-15 ) ) ;
#5448 = ORIENTED_EDGE ( 'NONE', *, *, #11297, .T. ) ;
#5449 = FACE_OUTER_BOUND ( 'NONE', #5157, .T. ) ;
#5450 = CARTESIAN_POINT ( 'NONE',  ( -49.86468353124999453, 41.95937500034138878, 16.20201782572377525 ) ) ;
#5451 = VECTOR ( 'NONE', #11154, 1000.000000000000000 ) ;
#5452 = DIRECTION ( 'NONE',  ( 0.000000000000000000, 0.000000000000000000, 1.000000000000000000 ) ) ;
#5453 = CARTESIAN_POINT ( 'NONE',  ( 26.23306594128796121, 283.6958662468466059, 4.966131882590526736 ) ) ;
#5454 = CARTESIAN_POINT ( 'NONE',  ( -22.46613188259093974, 283.6958662468269949, 8.733065941307639690 ) ) ;
#5455 = CARTESIAN_POINT ( 'NONE',  ( 40.34137639590981195, 33.12187500034139731, -29.30972558990011834 ) ) ;
#5456 = CARTESIAN_POINT ( 'NONE',  ( 30.81806926056962936, 37.15937500034139163, -42.41743335407646498 ) ) ;
#5457 = DIRECTION ( 'NONE',  ( 0.9777979793268667397, 0.2095497831645171394, -0.000000000000000000 ) ) ;
#5458 =( BOUNDED_CURVE ( )  B_SPLINE_CURVE ( 2, ( #6911, #12129, #5736, #13291, #11965, #1892, #10885, #10964, #561, #7153, #5903, #4570, #14686 ),
 .UNSPECIFIED., .F., .F. ) 
 B_SPLINE_CURVE_WITH_KNOTS ( ( 3, 2, 2, 2, 2, 2, 3 ),
 ( 0.4166666666666666852, 0.4199999999999999845, 0.4266666666666666941, 0.4333333333333333481, 0.4400000000000000022, 0.4466666666666666563, 0.4500000000000000111 ),
 .UNSPECIFIED. ) 
 CURVE ( )  GEOMETRIC_REPRESENTATION_ITEM ( )  RATIONAL_B_SPLINE_CURVE ( ( 0.9755282581475768211, 0.9755282581475770431, 1.000000000000000000, 0.9510565162951535312, 1.000000000000000000, 0.9510565162951535312, 1.000000000000000000, 0.9510565162951535312, 1.000000000000000000, 0.9510565162951535312, 1.000000000000000000, 0.9755282581475765991, 0.9755282581475768211 ) ) 
 REPRESENTATION_ITEM ( '' )  );
#5459 = CARTESIAN_POINT ( 'NONE',  ( -40.45084971874737789, 41.80000000000000426, -29.38926261462365730 ) ) ;
#5460 = EDGE_CURVE ( 'NONE', #2743, #9602, #10755, .T. ) ;
#5461 = CARTESIAN_POINT ( 'NONE',  ( 9.657523855033129090E-15, 22.28125000068279959, 52.57311121191334990 ) ) ;
#5462 = CARTESIAN_POINT ( 'NONE',  ( -15.40903463028480580, 44.32187500034140015, 47.42413220539094709 ) ) ;
#5463 = VECTOR ( 'NONE', #12791, 1000.000000000000000 ) ;
#5464 = CARTESIAN_POINT ( 'NONE',  ( -49.86468353124999453, 27.82187500034139305, -16.20201782572375393 ) ) ;
#5465 = CARTESIAN_POINT ( 'NONE',  ( -3.210462471511496205E-15, 47.35937500034138736, -52.43083105670540789 ) ) ;
#5466 = ORIENTED_EDGE ( 'NONE', *, *, #9680, .T. ) ;
#5467 = CARTESIAN_POINT ( 'NONE',  ( 15.45084971874737789, 38.38125000068279746, 47.55282581475767500 ) ) ;
#5468 = VERTEX_POINT ( 'NONE', #2408 ) ;
#5469 = CARTESIAN_POINT ( 'NONE',  ( -15.40544456622763470, 14.18301270189214947, 101.0000000000000000 ) ) ;
#5470 = DIRECTION ( 'NONE',  ( -0.000000000000000000, -1.000000000000000000, -0.000000000000000000 ) ) ;
#5471 = CIRCLE ( 'NONE', #4129, 16.50000000000000711 ) ;
#5472 = CARTESIAN_POINT ( 'NONE',  ( 4.126043002969939977, 5.493361027597405410, 101.0000000000000000 ) ) ;
#5473 = CARTESIAN_POINT ( 'NONE',  ( -15.40903463028480580, 44.32187500034140015, 47.42413220539094709 ) ) ;
#5474 = CARTESIAN_POINT ( 'NONE',  ( -30.81806926056963292, 25.55937500034139376, -42.41743335407647209 ) ) ;
#5475 = CARTESIAN_POINT ( 'NONE',  ( -40.45084971874737789, 39.58125000068280031, -29.38926261462365730 ) ) ;
#5476 = CARTESIAN_POINT ( 'NONE',  ( -49.86468353125000164, 39.92187500034139447, 0.000000000000000000 ) ) ;
#5477 = APPLICATION_PROTOCOL_DEFINITION ( 'draft international standard', 'automotive_design', 1998, #15229 ) ;
#5478 = DIRECTION ( 'NONE',  ( -0.000000000000000000, -1.000000000000000000, -0.000000000000000000 ) ) ;
#5479 = CARTESIAN_POINT ( 'NONE',  ( 40.34137639590981195, 45.12187500034139731, -29.30972558990011834 ) ) ;
#5480 = CYLINDRICAL_SURFACE ( 'NONE', #14924, 60.00000000000000711 ) ;
#5481 = CIRCLE ( 'NONE', #13419, 40.00000000000000000 ) ;
#5482 = ORIENTED_EDGE ( 'NONE', *, *, #10, .F. ) ;
#5483 = CIRCLE ( 'NONE', #13173, 17.50000000000000000 ) ;
#5484 = CARTESIAN_POINT ( 'NONE',  ( -15.40903463028481646, 21.45937500034139589, -47.42413220539093999 ) ) ;
#5485 = ORIENTED_EDGE ( 'NONE', *, *, #9175, .T. ) ;
#5486 = CARTESIAN_POINT ( 'NONE',  ( -7.919222016226816763, 45.33250428222963535, -49.99999999999999289 ) ) ;
#5487 = EDGE_LOOP ( 'NONE', ( #15628, #3760, #6506, #2705 ) ) ;
#5488 =( GEOMETRIC_REPRESENTATION_CONTEXT ( 3 ) GLOBAL_UNCERTAINTY_ASSIGNED_CONTEXT ( ( #12067 ) ) GLOBAL_UNIT_ASSIGNED_CONTEXT ( ( #2386, #13690, #16444 ) ) REPRESENTATION_CONTEXT ( 'NONE', 'WORKASPACE' ) );
#5489 = EDGE_CURVE ( 'NONE', #3882, #12433, #11316, .T. ) ;
#5490 = ADVANCED_FACE ( 'NONE', ( #3584 ), #217, .F. ) ;
#5491 = CARTESIAN_POINT ( 'NONE',  ( -13.33959974903384627, 33.83821319854129683, 102.0000000000000142 ) ) ;
#5492 = DIRECTION ( 'NONE',  ( -0.000000000000000000, 1.000000000000000000, -0.000000000000000000 ) ) ;
#5493 = DIRECTION ( 'NONE',  ( -0.000000000000000000, -1.000000000000000000, -0.000000000000000000 ) ) ;
#5494 = CARTESIAN_POINT ( 'NONE',  ( -15.45084971874737256, 23.60000000000000142, -47.55282581475767500 ) ) ;
#5495 = VECTOR ( 'NONE', #8882, 1000.000000000000114 ) ;
#5496 = CARTESIAN_POINT ( 'NONE',  ( -49.86468353125000164, 43.85937500034140157, 0.000000000000000000 ) ) ;
#5497 = AXIS2_PLACEMENT_3D ( 'NONE', #8426, #13569, #11097 ) ;
#5498 = CIRCLE ( 'NONE', #14753, 40.00000000000000000 ) ;
#5499 = DIRECTION ( 'NONE',  ( -0.8660254037844399289, 0.000000000000000000, -0.4999999999999978351 ) ) ;
#5500 = FACE_OUTER_BOUND ( 'NONE', #15959, .T. ) ;
#5501 = VECTOR ( 'NONE', #4780, 999.9999999999998863 ) ;
#5502 = CYLINDRICAL_SURFACE ( 'NONE', #14245, 50.00000000000000000 ) ;
#5503 =( NAMED_UNIT ( * ) PLANE_ANGLE_UNIT ( ) SI_UNIT ( $, .RADIAN. ) );
#5504 = CARTESIAN_POINT ( 'NONE',  ( 50.00000000000000000, 49.00000000000000000, -6.123233995736766085E-15 ) ) ;
#5505 = CARTESIAN_POINT ( 'NONE',  ( -50.00000000000000000, 39.78125000068279604, 0.000000000000000000 ) ) ;
#5506 = CARTESIAN_POINT ( 'NONE',  ( -7.919222016226870942, 38.22999571913595673, 49.99999999999997158 ) ) ;
#5507 = CARTESIAN_POINT ( 'NONE',  ( 15.45084971874737789, 46.38125000068279746, 47.55282581475767500 ) ) ;
#5508 = CYLINDRICAL_SURFACE ( 'NONE', #13598, 5.000000000000000000 ) ;
#5509 = EDGE_CURVE ( 'NONE', #8227, #1042, #3627, .T. ) ;
#5510 = ORIENTED_EDGE ( 'NONE', *, *, #6123, .T. ) ;
#5511 = CARTESIAN_POINT ( 'NONE',  ( 49.86468353125001585, 38.75937500034139305, 16.20201782572375038 ) ) ;
#5512 = ORIENTED_EDGE ( 'NONE', *, *, #3926, .F. ) ;
#5513 = EDGE_LOOP ( 'NONE', ( #1743, #16277, #14277, #4657 ) ) ;
#5514 = AXIS2_PLACEMENT_3D ( 'NONE', #15634, #4259, #9325 ) ;
#5515 = CARTESIAN_POINT ( 'NONE',  ( 30.90169943749474157, 49.08125000068280031, -42.53254041760200721 ) ) ;
#5516 = LINE ( 'NONE', #9246, #6842 ) ;
#5517 = CARTESIAN_POINT ( 'NONE',  ( 15.40903463028481113, 25.25937500034139660, -47.42413220539094709 ) ) ;
#5518 = EDGE_LOOP ( 'NONE', ( #1661, #1137, #2119, #5851 ) ) ;
#5519 = FACE_OUTER_BOUND ( 'NONE', #6364, .T. ) ;
#5520 = CARTESIAN_POINT ( 'NONE',  ( 50.00000000000000711, 34.89999999999999858, 16.24598481164530739 ) ) ;
#5521 = CARTESIAN_POINT ( 'NONE',  ( 11.92169313911843354, 33.90715708214350599, 102.0000000000000142 ) ) ;
#5522 = CARTESIAN_POINT ( 'NONE',  ( 15.40903463028481113, 27.32187500034139660, -47.42413220539094709 ) ) ;
#5523 = EDGE_CURVE ( 'NONE', #9777, #8525, #3673, .T. ) ;
#5524 = CARTESIAN_POINT ( 'NONE',  ( -49.99999999999999289, 37.88125000068279746, 16.24598481164533226 ) ) ;
#5525 = AXIS2_PLACEMENT_3D ( 'NONE', #3429, #1996, #13555 ) ;
#5526 = DIRECTION ( 'NONE',  ( -0.000000000000000000, -1.000000000000000000, -0.000000000000000000 ) ) ;
#5527 = CARTESIAN_POINT ( 'NONE',  ( -46.62157290631127893, 20.00000000000001066, 17.69020581817094850 ) ) ;
#5528 = CARTESIAN_POINT ( 'NONE',  ( 40.34137639590981195, 29.12187500034139376, -29.30972558990011834 ) ) ;
#5529 = AXIS2_PLACEMENT_3D ( 'NONE', #2813, #5575, #11635 ) ;
#5530 = CARTESIAN_POINT ( 'NONE',  ( -30.90169943749474513, 21.69999999999999574, -42.53254041760200721 ) ) ;
#5531 = CARTESIAN_POINT ( 'NONE',  ( -15.45084971874737256, 35.60000000000000142, -47.55282581475767500 ) ) ;
#5532 = CARTESIAN_POINT ( 'NONE',  ( 30.81806926056964002, 30.55937500034139731, 42.41743335407647209 ) ) ;
#5533 = EDGE_CURVE ( 'NONE', #16246, #9095, #12555, .T. ) ;
#5534 = DIRECTION ( 'NONE',  ( -1.000000000000000000, 0.000000000000000000, 0.000000000000000000 ) ) ;
#5535 = ORIENTED_EDGE ( 'NONE', *, *, #8930, .T. ) ;
#5536 = EDGE_CURVE ( 'NONE', #5162, #1062, #685, .T. ) ;
#5537 = CARTESIAN_POINT ( 'NONE',  ( 15.40903463028481113, 29.25937500034139660, -47.42413220539094709 ) ) ;
#5538 = VECTOR ( 'NONE', #15538, 1000.000000000000000 ) ;
#5539 = ORIENTED_EDGE ( 'NONE', *, *, #9567, .F. ) ;
#5540 = LINE ( 'NONE', #4280, #4163 ) ;
#5541 = CARTESIAN_POINT ( 'NONE',  ( 30.81806926056964002, 44.55937500034139020, 42.41743335407647209 ) ) ;
#5542 = CARTESIAN_POINT ( 'NONE',  ( -40.45084971874737079, 38.20000000000000284, 29.38926261462367151 ) ) ;
#5543 = CARTESIAN_POINT ( 'NONE',  ( -49.86468353125000164, 19.92187500034139447, 0.000000000000000000 ) ) ;
#5544 = CARTESIAN_POINT ( 'NONE',  ( -24.96465690379244862, 286.9981936728224241, 7.464656903793317255 ) ) ;
#5545 = CARTESIAN_POINT ( 'NONE',  ( 49.86468353125000164, 38.92187500034139447, -6.106662507704105588E-15 ) ) ;
#5546 = CARTESIAN_POINT ( 'NONE',  ( -49.86468353124999453, 35.95937500034139589, 16.20201782572377169 ) ) ;
#5547 = CARTESIAN_POINT ( 'NONE',  ( 5.000000000000000000, 90.58578643762692195, -1.414213562373097588 ) ) ;
#5548 = CARTESIAN_POINT ( 'NONE',  ( -30.90169943749474868, 41.70000000000000284, -42.53254041760200721 ) ) ;
#5549 = CARTESIAN_POINT ( 'NONE',  ( 30.81806926056964002, 48.55937500034138310, 42.41743335407647209 ) ) ;
#5550 = CARTESIAN_POINT ( 'NONE',  ( 15.40903463028481113, 45.32187500034140015, -47.42413220539094709 ) ) ;
#5551 = CARTESIAN_POINT ( 'NONE',  ( 49.86468353125000164, 24.92187500034139802, -6.106662507704105588E-15 ) ) ;
#5552 = ADVANCED_FACE ( 'NONE', ( #540 ), #3040, .T. ) ;
#5553 = CARTESIAN_POINT ( 'NONE',  ( -3.111920190527341144E-15, 27.28125000068279604, -50.00000000000000000 ) ) ;
#5554 = ORIENTED_EDGE ( 'NONE', *, *, #787, .T. ) ;
#5555 = CARTESIAN_POINT ( 'NONE',  ( -50.00000000000000000, 29.78125000068279959, 0.000000000000000000 ) ) ;
#5556 = AXIS2_PLACEMENT_3D ( 'NONE', #2209, #7306, #3887 ) ;
#5557 = ORIENTED_EDGE ( 'NONE', *, *, #6127, .F. ) ;
#5558 = DIRECTION ( 'NONE',  ( -0.000000000000000000, -1.000000000000000000, -0.000000000000000000 ) ) ;
#5559 = CARTESIAN_POINT ( 'NONE',  ( 15.39925740754319605, 14.18658485962441240, 101.0000000000000000 ) ) ;
#5560 = SHAPE_REPRESENTATION ( 'Lid Filler Cap _ Measuring Cup', ( #15812 ), #5488 ) ;
#5561 = CARTESIAN_POINT ( 'NONE',  ( 50.00000000000000711, 30.68125000068279462, 16.24598481164530739 ) ) ;
#5562 = CARTESIAN_POINT ( 'NONE',  ( 30.81806926056964002, 44.62187500034139731, 42.41743335407646498 ) ) ;
#5563 = CARTESIAN_POINT ( 'NONE',  ( 15.40903463028481113, 27.25937500034139660, -47.42413220539094709 ) ) ;
#5564 = DIRECTION ( 'NONE',  ( -1.000000000000000000, 0.000000000000000000, 0.000000000000000000 ) ) ;
#5565 = CARTESIAN_POINT ( 'NONE',  ( -15.40903463028481646, 41.52187500034139589, -47.42413220539093999 ) ) ;
#5566 = CARTESIAN_POINT ( 'NONE',  ( 0.000000000000000000, 0.000000000000000000, 0.000000000000000000 ) ) ;
#5567 = EDGE_CURVE ( 'NONE', #7399, #8881, #15926, .T. ) ;
#5568 = CARTESIAN_POINT ( 'NONE',  ( -49.86468353125000164, 43.92187500034140157, 0.000000000000000000 ) ) ;
#5569 = EDGE_CURVE ( 'NONE', #12110, #11124, #15754, .T. ) ;
#5570 = DIRECTION ( 'NONE',  ( 0.8660254037844327124, 0.000000000000000000, -0.5000000000000103251 ) ) ;
#5571 = ORIENTED_EDGE ( 'NONE', *, *, #9953, .F. ) ;
#5572 = CARTESIAN_POINT ( 'NONE',  ( -49.86468353125000164, 43.92187500034140157, 0.000000000000000000 ) ) ;
#5573 = EDGE_LOOP ( 'NONE', ( #3925, #13135, #6838, #2186, #11428 ) ) ;
#5574 = ORIENTED_EDGE ( 'NONE', *, *, #5489, .T. ) ;
#5575 = DIRECTION ( 'NONE',  ( -1.000000000000000000, 0.000000000000000000, 0.000000000000000000 ) ) ;
#5576 = DIRECTION ( 'NONE',  ( -0.000000000000000000, -1.000000000000000000, -0.000000000000000000 ) ) ;
#5577 = DIRECTION ( 'NONE',  ( 0.000000000000000000, -0.000000000000000000, -1.000000000000000000 ) ) ;
#5578 = CARTESIAN_POINT ( 'NONE',  ( 30.90169943749474157, 23.29999999999999716, -42.53254041760200721 ) ) ;
#5579 = CARTESIAN_POINT ( 'NONE',  ( 15.40903463028481113, 45.25937500034140015, -47.42413220539094709 ) ) ;
#5580 = CARTESIAN_POINT ( 'NONE',  ( -15.45084971874736368, 32.18125000068279462, 47.55282581475768211 ) ) ;
#5581 = CARTESIAN_POINT ( 'NONE',  ( 0.000000000000000000, 52.00000000000000711, 0.000000000000000000 ) ) ;
#5582 = PLANE ( 'NONE',  #3292 ) ;
#5583 = CARTESIAN_POINT ( 'NONE',  ( 50.00000000000000000, 36.78125000068280315, -6.123233995736766085E-15 ) ) ;
#5584 = CARTESIAN_POINT ( 'NONE',  ( -40.45084971874737789, 37.58125000068280031, -29.38926261462365730 ) ) ;
#5585 = CARTESIAN_POINT ( 'NONE',  ( 30.90169943749475223, 20.48125000068279178, 42.53254041760199300 ) ) ;
#5586 = CARTESIAN_POINT ( 'NONE',  ( -7.300484685133206142, 37.66786040234655530, 101.6666710451724214 ) ) ;
#5587 = ORIENTED_EDGE ( 'NONE', *, *, #13322, .T. ) ;
#5588 = CARTESIAN_POINT ( 'NONE',  ( 30.81806926056964002, 34.55937500034139731, 42.41743335407647209 ) ) ;
#5589 = AXIS2_PLACEMENT_3D ( 'NONE', #9549, #631, #389 ) ;
#5590 = ORIENTED_EDGE ( 'NONE', *, *, #16177, .F. ) ;
#5591 = ORIENTED_EDGE ( 'NONE', *, *, #2216, .F. ) ;
#5592 = FACE_BOUND ( 'NONE', #206, .T. ) ;
#5593 = DIRECTION ( 'NONE',  ( 5.069245582283711292E-17, 1.000000000000000000, -8.780190904559502465E-17 ) ) ;
#5594 = CARTESIAN_POINT ( 'NONE',  ( 30.81806926056962936, 23.15937500034139873, -42.41743335407647209 ) ) ;
#5595 = EDGE_LOOP ( 'NONE', ( #5590, #6125, #9604, #9587 ) ) ;
#5596 = CARTESIAN_POINT ( 'NONE',  ( 8.446640517145639571E-15, 48.49999999999999289, 50.00000000000000000 ) ) ;
#5597 = CARTESIAN_POINT ( 'NONE',  ( 7.919222016226940219, 23.44874571845315359, -49.99999999999996447 ) ) ;
#5598 = CARTESIAN_POINT ( 'NONE',  ( 20.00000000000000355, 284.0710678118655323, 7.500000000000000000 ) ) ;
#5599 = CARTESIAN_POINT ( 'NONE',  ( -49.86468353124999453, 30.02187500034139234, 16.20201782572377169 ) ) ;
#5600 = CARTESIAN_POINT ( 'NONE',  ( -14.26268078651477822, 98.74453744460426208, 5.000000000000000000 ) ) ;
#5601 = CARTESIAN_POINT ( 'NONE',  ( 8.446640517145639571E-15, 26.50000000000000000, 50.00000000000000000 ) ) ;
#5602 = CARTESIAN_POINT ( 'NONE',  ( -49.86468353124999453, 22.02187500034139589, 16.20201782572377169 ) ) ;
#5603 = DIRECTION ( 'NONE',  ( 0.000000000000000000, -1.000000000000000000, 0.000000000000000000 ) ) ;
#5604 = CARTESIAN_POINT ( 'NONE',  ( 9.657523855033129090E-15, 32.50000000000000000, 52.57311121191334990 ) ) ;
#5605 = CARTESIAN_POINT ( 'NONE',  ( 49.86468353125001585, 34.75937500034139305, 16.20201782572375038 ) ) ;
#5606 = DIRECTION ( 'NONE',  ( -0.2079116908177665590, 0.9781476007338041345, 0.000000000000000000 ) ) ;
#5607 = VERTEX_POINT ( 'NONE', #4305 ) ;
#5608 = ADVANCED_FACE ( 'NONE', ( #9369 ), #13269, .T. ) ;
#5609 = CARTESIAN_POINT ( 'NONE',  ( 49.86468353125001585, 32.75937500034140015, 16.20201782572375038 ) ) ;
#5610 = ORIENTED_EDGE ( 'NONE', *, *, #8539, .F. ) ;
#5611 = CARTESIAN_POINT ( 'NONE',  ( 0.000000000000000000, 53.82568851450475478, 0.000000000000000000 ) ) ;
#5612 = CARTESIAN_POINT ( 'NONE',  ( -49.86468353124999453, 43.95937500034138878, 16.20201782572377525 ) ) ;
#5613 = CARTESIAN_POINT ( 'NONE',  ( 24.98849325795415055, 282.6608420050615678, 9.994246628976808822 ) ) ;
#5614 = ADVANCED_FACE ( 'NONE', ( #4548 ), #7827, .T. ) ;
#5615 = ADVANCED_FACE ( 'NONE', ( #14347 ), #4382, .T. ) ;
#5616 = CARTESIAN_POINT ( 'NONE',  ( -26.69586624682724718, 283.2330659413073590, 5.891732493678457416 ) ) ;
#5617 = CARTESIAN_POINT ( 'NONE',  ( -30.81806926056963292, 37.62187500034139020, -42.41743335407647209 ) ) ;
#5618 = CARTESIAN_POINT ( 'NONE',  ( 15.40903463028481113, 37.25937500034140015, -47.42413220539094709 ) ) ;
#5619 = CARTESIAN_POINT ( 'NONE',  ( -6.661118525005218949, 38.69041383028340420, 101.0000000000000000 ) ) ;
#5620 = CARTESIAN_POINT ( 'NONE',  ( -49.99999999999999289, 39.90000000000001279, -16.24598481164531449 ) ) ;
#5621 = PRODUCT ( 'Rubber Leak-Proof Gasket Ring', 'Rubber Leak-Proof Gasket Ring', '', ( #10375 ) ) ;
#5622 = EDGE_CURVE ( 'NONE', #16014, #3621, #3941, .T. ) ;
#5623 = CARTESIAN_POINT ( 'NONE',  ( -40.45084971874737789, 21.58125000068279675, -29.38926261462365730 ) ) ;
#5624 = CARTESIAN_POINT ( 'NONE',  ( -49.86468353125000164, 43.92187500034140157, 0.000000000000000000 ) ) ;
#5625 = CARTESIAN_POINT ( 'NONE',  ( -30.81806926056962226, 30.22187500034139518, 42.41743335407647919 ) ) ;
#5626 = CARTESIAN_POINT ( 'NONE',  ( 49.86468353125000164, 46.85937500034139447, -6.106662507704105588E-15 ) ) ;
#5627 = VERTEX_POINT ( 'NONE', #6888 ) ;
#5628 = CARTESIAN_POINT ( 'NONE',  ( -40.45084971874737789, 29.58125000068279675, -29.38926261462365730 ) ) ;
#5629 = ORIENTED_EDGE ( 'NONE', *, *, #13441, .F. ) ;
#5630 = FACE_OUTER_BOUND ( 'NONE', #1976, .T. ) ;
#5631 = DIRECTION ( 'NONE',  ( 0.000000000000000000, 1.000000000000000000, 0.000000000000000000 ) ) ;
#5632 = CARTESIAN_POINT ( 'NONE',  ( -40.34137639590981905, 41.72187500034139873, -29.30972558990011478 ) ) ;
#5633 = CARTESIAN_POINT ( 'NONE',  ( -15.40903463028481646, 25.45937500034139589, -47.42413220539093999 ) ) ;
#5634 = CARTESIAN_POINT ( 'NONE',  ( -7.919222016226752814, 39.33250428222963535, -50.00000000000000711 ) ) ;
#5635 = CARTESIAN_POINT ( 'NONE',  ( -30.81806926056962226, 44.22187500034139163, 42.41743335407647919 ) ) ;
#5636 = CARTESIAN_POINT ( 'NONE',  ( -2.445080149700054274E-14, 46.28125000068280315, 50.00000000000000000 ) ) ;
#5637 = ORIENTED_EDGE ( 'NONE', *, *, #14308, .F. ) ;
#5638 = CARTESIAN_POINT ( 'NONE',  ( -15.40903463028481646, 41.52187500034139589, -47.42413220539093999 ) ) ;
#5639 = ORIENTED_EDGE ( 'NONE', *, *, #12767, .T. ) ;
#5640 = EDGE_LOOP ( 'NONE', ( #4761, #3706, #14775, #10156 ) ) ;
#5641 =( BOUNDED_CURVE ( )  B_SPLINE_CURVE ( 3, ( #11492, #5284, #4015, #6186 ),
 .UNSPECIFIED., .F., .T. ) 
 B_SPLINE_CURVE_WITH_KNOTS ( ( 4, 4 ),
 ( 2.558501865821646959, 3.141592653589793116 ),
 .UNSPECIFIED. ) 
 CURVE ( )  GEOMETRIC_REPRESENTATION_ITEM ( )  RATIONAL_B_SPLINE_CURVE ( ( 1.000000000000000000, 0.9718672150731668680, 0.9718672150731668680, 1.000000000000000000 ) ) 
 REPRESENTATION_ITEM ( '' )  );
#5642 = B_SPLINE_CURVE_WITH_KNOTS ( 'NONE', 3,
 ( #2808, #1562, #6656, #11537 ),
 .UNSPECIFIED., .F., .F.,
 ( 4, 4 ),
 ( 0.01140363079879802566, 0.01281815069648909247 ),
 .UNSPECIFIED. ) ;
#5643 = FACE_OUTER_BOUND ( 'NONE', #3373, .T. ) ;
#5644 = CARTESIAN_POINT ( 'NONE',  ( 40.45084971874737079, 38.98125000068279888, -29.38926261462366440 ) ) ;
#5645 = CARTESIAN_POINT ( 'NONE',  ( 6.123233995736766085E-15, 20.00000000000000355, -50.00000000000000000 ) ) ;
#5646 = CARTESIAN_POINT ( 'NONE',  ( -30.90169943749473802, 24.29999999999999716, 42.53254041760200721 ) ) ;
#5647 = CARTESIAN_POINT ( 'NONE',  ( -40.34137639590981195, 46.05937500034139731, 29.30972558990012189 ) ) ;
#5648 = CARTESIAN_POINT ( 'NONE',  ( -8.880528407616480990, 25.91118970470954963, 102.0000000000000142 ) ) ;
#5649 = DIRECTION ( 'NONE',  ( 0.4999999999999919509, 0.8660254037844432595, 0.000000000000000000 ) ) ;
#5650 = CARTESIAN_POINT ( 'NONE',  ( -30.90169943749473447, 34.08125000068279320, 42.53254041760200721 ) ) ;
#5651 = CARTESIAN_POINT ( 'NONE',  ( -24.78626291527393732, 25.00000000000000355, -5.650101528493794767 ) ) ;
#5652 = DIRECTION ( 'NONE',  ( -0.7431448254773860285, -0.6691306063588672304, 0.000000000000000000 ) ) ;
#5653 = AXIS2_PLACEMENT_3D ( 'NONE', #6568, #11626, #11701 ) ;
#5654 = CARTESIAN_POINT ( 'NONE',  ( 0.000000000000000000, 50.00000000000000000, 0.000000000000000000 ) ) ;
#5655 = EDGE_CURVE ( 'NONE', #7759, #7784, #8060, .T. ) ;
#5656 = CARTESIAN_POINT ( 'NONE',  ( 5.000000000000000000, 92.00000000000001421, 0.000000000000000000 ) ) ;
#5657 = ORIENTED_EDGE ( 'NONE', *, *, #15569, .T. ) ;
#5658 = CARTESIAN_POINT ( 'NONE',  ( -49.86468353124999453, 29.75937500034139305, -16.20201782572375393 ) ) ;
#5659 = ORIENTED_EDGE ( 'NONE', *, *, #7269, .T. ) ;
#5660 = ORIENTED_EDGE ( 'NONE', *, *, #4641, .F. ) ;
#5661 = VERTEX_POINT ( 'NONE', #6964 ) ;
#5662 = CARTESIAN_POINT ( 'NONE',  ( 7.513064459987437071E-14, 42.50000000000000000, 50.00000000000000000 ) ) ;
#5663 = CARTESIAN_POINT ( 'NONE',  ( -3.750000000000069278, 40.00000000000000711, -6.495190528383228745 ) ) ;
#5664 = CARTESIAN_POINT ( 'NONE',  ( -30.81806926056963292, 25.55937500034139376, -42.41743335407647209 ) ) ;
#5666 = ORIENTED_EDGE ( 'NONE', *, *, #2651, .F. ) ;
#5665 = VECTOR ( 'NONE', #3522, 1000.000000000000000 ) ;
#5667 = CARTESIAN_POINT ( 'NONE',  ( 16.79120288457601262, 27.43006142852259899, 101.0000000000000000 ) ) ;
#5668 = LINE ( 'NONE', #10735, #13955 ) ;
#5669 = LINE ( 'NONE', #2843, #5144 ) ;
#5670 = CARTESIAN_POINT ( 'NONE',  ( 30.81806926056962936, 27.22187500034139518, -42.41743335407646498 ) ) ;
#5671 = CARTESIAN_POINT ( 'NONE',  ( 7.919222016226875382, 39.44874571845315359, -49.99999999999997158 ) ) ;
#5672 = CARTESIAN_POINT ( 'NONE',  ( 16.94295052416147840, 17.97534012751635402, 95.33699471030656980 ) ) ;
#5673 = DIRECTION ( 'NONE',  ( 1.224646799147353207E-16, -1.000000000000000000, 0.000000000000000000 ) ) ;
#5674 = CARTESIAN_POINT ( 'NONE',  ( 40.34137639590981905, 20.72187500034139873, 29.30972558990010768 ) ) ;
#5675 = CARTESIAN_POINT ( 'NONE',  ( 9.234334497652928468E-15, 101.0808929720139702, -9.080892972013931086 ) ) ;
#5676 = CARTESIAN_POINT ( 'NONE',  ( -3.219174618344376363E-15, 37.50000000000000000, -52.57311121191334990 ) ) ;
#5677 = CARTESIAN_POINT ( 'NONE',  ( 49.86468353124999453, 24.95937500034139234, -16.20201782572376459 ) ) ;
#5678 = VECTOR ( 'NONE', #502, 1000.000000000000000 ) ;
#5679 = CARTESIAN_POINT ( 'NONE',  ( -2.547328955960238000E-13, 30.49999999999999645, 49.99999999999999289 ) ) ;
#5680 = ORIENTED_EDGE ( 'NONE', *, *, #2226, .T. ) ;
#5681 = CARTESIAN_POINT ( 'NONE',  ( -49.86468353124999453, 31.95937500034139944, 16.20201782572377169 ) ) ;
#5682 = ORIENTED_EDGE ( 'NONE', *, *, #3555, .T. ) ;
#5683 = DIRECTION ( 'NONE',  ( -0.3420201433256697121, 0.6644630243886755494, 0.6644630243886733290 ) ) ;
#5684 = CARTESIAN_POINT ( 'NONE',  ( -15.40903463028481646, 39.45937500034139589, -47.42413220539093999 ) ) ;
#5685 = EDGE_CURVE ( 'NONE', #7461, #960, #3050, .T. ) ;
#5686 = CARTESIAN_POINT ( 'NONE',  ( 26.77784341583515371, 282.2553694771634696, 10.88892170791772251 ) ) ;
#5687 = VECTOR ( 'NONE', #10828, 1000.000000000000000 ) ;
#5688 = AXIS2_PLACEMENT_3D ( 'NONE', #3810, #1218, #15022 ) ;
#5689 = CARTESIAN_POINT ( 'NONE',  ( -5.026048470455357631, 37.52604847045536474, -39.76282541253124947 ) ) ;
#5690 = CARTESIAN_POINT ( 'NONE',  ( 40.34137639590981195, 29.12187500034139376, -29.30972558990011834 ) ) ;
#5691 = CARTESIAN_POINT ( 'NONE',  ( -15.40903463028480580, 38.25937500034140015, 47.42413220539094709 ) ) ;
#5692 = CARTESIAN_POINT ( 'NONE',  ( 4.320770838041294581, 30.97531352606685218, 101.0000000000000000 ) ) ;
#5693 = CARTESIAN_POINT ( 'NONE',  ( -49.86468353124999453, 30.02187500034139234, 16.20201782572377525 ) ) ;
#5694 = CARTESIAN_POINT ( 'NONE',  ( 40.45084971874737079, 39.19999999999999574, -29.38926261462366440 ) ) ;
#5695 = CARTESIAN_POINT ( 'NONE',  ( 30.81806926056962936, 47.15937500034138452, -42.41743335407647209 ) ) ;
#5696 = CARTESIAN_POINT ( 'NONE',  ( 49.86468353125001585, 42.82187500034139305, 16.20201782572375038 ) ) ;
#5697 = CARTESIAN_POINT ( 'NONE',  ( 50.00000000000000000, 49.00000000000000000, -6.123233995736766085E-15 ) ) ;
#5698 = EDGE_CURVE ( 'NONE', #11702, #7069, #12017, .T. ) ;
#5699 = PRODUCT_DEFINITION ( 'UNKNOWN', '', #16346, #8415 ) ;
#5700 = VERTEX_POINT ( 'NONE', #10781 ) ;
#5701 = VECTOR ( 'NONE', #1359, 1000.000000000000000 ) ;
#5702 = DIRECTION ( 'NONE',  ( -1.000000000000000000, 0.000000000000000000, 0.000000000000000000 ) ) ;
#5703 = ORIENTED_EDGE ( 'NONE', *, *, #8203, .T. ) ;
#5704 = EDGE_LOOP ( 'NONE', ( #8739, #11969, #10484, #13439 ) ) ;
#5705 = CARTESIAN_POINT ( 'NONE',  ( 40.45084971874737079, 28.98125000068279888, -29.38926261462366440 ) ) ;
#5706 = ORIENTED_EDGE ( 'NONE', *, *, #6252, .T. ) ;
#5707 = ADVANCED_FACE ( 'NONE', ( #6725 ), #10545, .T. ) ;
#5708 = CARTESIAN_POINT ( 'NONE',  ( 0.000000000000000000, 262.0000000000000000, -45.00000000000000711 ) ) ;
#5709 = CARTESIAN_POINT ( 'NONE',  ( 30.90169943749475223, 30.48125000068279533, 42.53254041760199300 ) ) ;
#5710 = CARTESIAN_POINT ( 'NONE',  ( 49.86468353124999453, 39.02187500034138878, -16.20201782572376104 ) ) ;
#5711 = CARTESIAN_POINT ( 'NONE',  ( 9.631387414534489405E-15, 20.35937500034139092, 52.43083105670540789 ) ) ;
#5712 = DIRECTION ( 'NONE',  ( -0.6691306063588569053, -0.7431448254773954654, 0.000000000000000000 ) ) ;
#5713 = VECTOR ( 'NONE', #919, 1000.000000000000000 ) ;
#5714 = EDGE_CURVE ( 'NONE', #1840, #2524, #13106, .T. ) ;
#5715 = CARTESIAN_POINT ( 'NONE',  ( 15.45084971874737789, 36.60000000000000142, 47.55282581475767500 ) ) ;
#5716 = CARTESIAN_POINT ( 'NONE',  ( -49.86468353124999453, 42.02187500034139589, 16.20201782572377525 ) ) ;
#5717 = CARTESIAN_POINT ( 'NONE',  ( 40.45084971874737079, 31.20000000000000284, -29.38926261462366440 ) ) ;
#5718 = ORIENTED_EDGE ( 'NONE', *, *, #3167, .T. ) ;
#5719 = CARTESIAN_POINT ( 'NONE',  ( 9.631387414534489405E-15, 44.42187500034140157, 52.43083105670540789 ) ) ;
#5720 = ORIENTED_EDGE ( 'NONE', *, *, #2445, .T. ) ;
#5721 = ORIENTED_EDGE ( 'NONE', *, *, #2754, .T. ) ;
#5722 = EDGE_CURVE ( 'NONE', #10705, #8435, #13587, .T. ) ;
#5723 = ORIENTED_EDGE ( 'NONE', *, *, #6682, .T. ) ;
#5724 = CARTESIAN_POINT ( 'NONE',  ( -30.90169943749474513, 39.48125000068278467, -42.53254041760200721 ) ) ;
#5725 = CARTESIAN_POINT ( 'NONE',  ( 2.500000000000000000, 242.0000000000000284, -47.99999999999999289 ) ) ;
#5726 = DIRECTION ( 'NONE',  ( -0.000000000000000000, -1.000000000000000000, -0.000000000000000000 ) ) ;
#5727 = CARTESIAN_POINT ( 'NONE',  ( 1.293669679204937499E-13, 37.28125000068280315, -50.00000000000000000 ) ) ;
#5728 = CARTESIAN_POINT ( 'NONE',  ( 40.34137639590981195, 43.05937500034139731, -29.30972558990011834 ) ) ;
#5729 = CARTESIAN_POINT ( 'NONE',  ( -49.86468353125000164, 47.85937500034139447, 0.000000000000000000 ) ) ;
#5730 = DIRECTION ( 'NONE',  ( 0.000000000000000000, 1.000000000000000000, 0.000000000000000000 ) ) ;
#5731 = ADVANCED_FACE ( 'NONE', ( #3631 ), #14913, .F. ) ;
#5732 = DIRECTION ( 'NONE',  ( -0.8660254037844320463, 0.5000000000000113243, 0.000000000000000000 ) ) ;
#5733 = AXIS2_PLACEMENT_3D ( 'NONE', #13236, #15644, #15560 ) ;
#5734 = LINE ( 'NONE', #15869, #9670 ) ;
#5735 = FACE_OUTER_BOUND ( 'NONE', #6214, .T. ) ;
#5736 = CARTESIAN_POINT ( 'NONE',  ( 15.45084971874736723, 37.40000000000000568, -47.55282581475768211 ) ) ;
#5737 = ORIENTED_EDGE ( 'NONE', *, *, #13228, .T. ) ;
#5738 =( BOUNDED_CURVE ( )  B_SPLINE_CURVE ( 2, ( #10799, #3393, #14846, #2206, #3475, #964, #14673, #7302, #13523, #5724, #13358, #8531, #15860 ),
 .UNSPECIFIED., .F., .F. ) 
 B_SPLINE_CURVE_WITH_KNOTS ( ( 3, 2, 2, 2, 2, 2, 3 ),
 ( 0.3166666666666667074, 0.3200000000000000067, 0.3266666666666666607, 0.3333333333333333148, 0.3400000000000000244, 0.3466666666666666785, 0.3500000000000000333 ),
 .UNSPECIFIED. ) 
 CURVE ( )  GEOMETRIC_REPRESENTATION_ITEM ( )  RATIONAL_B_SPLINE_CURVE ( ( 0.9755282581475768211, 0.9755282581475770431, 1.000000000000000000, 0.9510565162951535312, 1.000000000000000000, 0.9510565162951535312, 1.000000000000000000, 0.9510565162951535312, 1.000000000000000000, 0.9510565162951535312, 1.000000000000000000, 0.9755282581475765991, 0.9755282581475768211 ) ) 
 REPRESENTATION_ITEM ( '' )  );
#5739 = CARTESIAN_POINT ( 'NONE',  ( 49.86468353125001585, 32.75937500034140015, 16.20201782572375038 ) ) ;
#5740 = ORIENTED_EDGE ( 'NONE', *, *, #3374, .F. ) ;
#5741 = EDGE_LOOP ( 'NONE', ( #6522, #5399, #11459, #264 ) ) ;
#5742 = ORIENTED_EDGE ( 'NONE', *, *, #1414, .F. ) ;
#5743 = EDGE_CURVE ( 'NONE', #12158, #12941, #12185, .T. ) ;
#5744 = CARTESIAN_POINT ( 'NONE',  ( -30.90169943749474868, 45.48125000068279178, -42.53254041760200721 ) ) ;
#5745 = VECTOR ( 'NONE', #13780, 1000.000000000000114 ) ;
#5746 = CIRCLE ( 'NONE', #14752, 14.08089297201391155 ) ;
#5747 = VECTOR ( 'NONE', #416, 1000.000000000000114 ) ;
#5748 = FACE_OUTER_BOUND ( 'NONE', #15173, .T. ) ;
#5749 = CARTESIAN_POINT ( 'NONE',  ( -40.34137639590981195, 22.05937500034139731, 29.30972558990012189 ) ) ;
#5750 = AXIS2_PLACEMENT_3D ( 'NONE', #14715, #8498, #6104 ) ;
#5751 = ORIENTED_EDGE ( 'NONE', *, *, #5909, .F. ) ;
#5752 = DIRECTION ( 'NONE',  ( -0.000000000000000000, 1.000000000000000000, -0.000000000000000000 ) ) ;
#5753 = CARTESIAN_POINT ( 'NONE',  ( -2.500000000000000000, 242.0000000000000284, -47.99999999999999289 ) ) ;
#5754 = FACE_BOUND ( 'NONE', #8286, .T. ) ;
#5755 = DIRECTION ( 'NONE',  ( 0.000000000000000000, 0.000000000000000000, -1.000000000000000000 ) ) ;
#5756 = CARTESIAN_POINT ( 'NONE',  ( 49.86468353125000164, 26.92187500034139802, -6.106662507704105588E-15 ) ) ;
#5757 = CARTESIAN_POINT ( 'NONE',  ( -15.45084971874736368, 48.40000000000000568, 47.55282581475768211 ) ) ;
#5758 = CARTESIAN_POINT ( 'NONE',  ( 7.919222016226875382, 37.22999571913595673, -49.99999999999997158 ) ) ;
#5759 = CARTESIAN_POINT ( 'NONE',  ( 20.00000000000000000, 312.0000000000000568, 2.500000000000002220 ) ) ;
#5760 = CARTESIAN_POINT ( 'NONE',  ( -49.86468353125000164, 21.92187500034139802, 0.000000000000000000 ) ) ;
#5761 = CARTESIAN_POINT ( 'NONE',  ( -5.000000000000000000, 30.31797207441543307, -38.93949884783829418 ) ) ;
#5762 = CARTESIAN_POINT ( 'NONE',  ( -30.90169943749474868, 37.70000000000000995, -42.53254041760200721 ) ) ;
#5763 = CARTESIAN_POINT ( 'NONE',  ( -49.86468353124999453, 25.95937500034139944, 16.20201782572377525 ) ) ;
#5764 = AXIS2_PLACEMENT_3D ( 'NONE', #7468, #6146, #8540 ) ;
#5765 = AXIS2_PLACEMENT_3D ( 'NONE', #843, #3598, #10002 ) ;
#5766 = CARTESIAN_POINT ( 'NONE',  ( -40.34137639590981905, 49.65937500034139873, -29.30972558990011478 ) ) ;
#5767 = EDGE_LOOP ( 'NONE', ( #13077, #3216, #12293, #1305 ) ) ;
#5768 = UNCERTAINTY_MEASURE_WITH_UNIT (LENGTH_MEASURE( 1.000000000000000082E-05 ), #1799, 'distance_accuracy_value', 'NONE');
#5769 = EDGE_LOOP ( 'NONE', ( #6079, #3944 ) ) ;
#5770 = CARTESIAN_POINT ( 'NONE',  ( 20.00000000000000000, 312.0000000000000568, -2.499999999999999556 ) ) ;
#5771 = CARTESIAN_POINT ( 'NONE',  ( 40.34137639590981195, 39.05937500034140442, -29.30972558990011834 ) ) ;
#5772 = EDGE_CURVE ( 'NONE', #16375, #4102, #6205, .T. ) ;
#5773 = VECTOR ( 'NONE', #14163, 1000.000000000000000 ) ;
#5774 = CARTESIAN_POINT ( 'NONE',  ( 30.90169943749473802, 29.08125000068280031, -42.53254041760200721 ) ) ;
#5775 = VECTOR ( 'NONE', #13442, 1000.000000000000000 ) ;
#5776 = FACE_OUTER_BOUND ( 'NONE', #12710, .T. ) ;
#5777 = CARTESIAN_POINT ( 'NONE',  ( 40.34137639590981905, 26.72187500034139518, 29.30972558990010768 ) ) ;
#5778 = CARTESIAN_POINT ( 'NONE',  ( -49.86468353125000164, 33.85937500034139447, 0.000000000000000000 ) ) ;
#5779 = CARTESIAN_POINT ( 'NONE',  ( 7.919222016226822092, 26.33250428222964246, 49.99999999999999289 ) ) ;
#5780 = CARTESIAN_POINT ( 'NONE',  ( 30.81806926056962936, 33.22187500034139163, -42.41743335407647209 ) ) ;
#5781 = CARTESIAN_POINT ( 'NONE',  ( -15.40903463028480580, 42.25937500034139305, 47.42413220539094709 ) ) ;
#5782 = CARTESIAN_POINT ( 'NONE',  ( 40.34137639590981195, 41.12187500034139731, -29.30972558990011834 ) ) ;
#5783 = CARTESIAN_POINT ( 'NONE',  ( -40.34137639590981195, 22.12187500034139731, 29.30972558990012189 ) ) ;
#5784 = ORIENTED_EDGE ( 'NONE', *, *, #1565, .F. ) ;
#5785 = CARTESIAN_POINT ( 'NONE',  ( 15.40903463028482356, 48.45937500034140299, 47.42413220539093999 ) ) ;
#5786 = ORIENTED_EDGE ( 'NONE', *, *, #4962, .F. ) ;
#5787 = EDGE_LOOP ( 'NONE', ( #15096, #4539, #2231, #13857, #12431, #7474, #13355, #11479, #15877, #12869, #9128, #16080, #12737, #14862, #4000, #5849, #6759, #14592, #9126, #3940, #3257, #12413, #8782, #304, #4409, #138, #7279, #10652, #6232 ) ) ;
#5788 = CARTESIAN_POINT ( 'NONE',  ( -50.00000000000000000, 31.78125000068279959, 0.000000000000000000 ) ) ;
#5789 = VERTEX_POINT ( 'NONE', #7127 ) ;
#5790 = CARTESIAN_POINT ( 'NONE',  ( 30.90169943749473802, 41.08125000068280031, -42.53254041760200721 ) ) ;
#5791 = CARTESIAN_POINT ( 'NONE',  ( 49.86468353124999453, 43.02187500034138878, -16.20201782572376104 ) ) ;
#5792 = CARTESIAN_POINT ( 'NONE',  ( -15.40903463028480580, 46.32187500034140015, 47.42413220539094709 ) ) ;
#5793 = ADVANCED_FACE ( 'NONE', ( #16003 ), #3542, .T. ) ;
#5794 = DIRECTION ( 'NONE',  ( 0.000000000000000000, 0.000000000000000000, 1.000000000000000000 ) ) ;
#5795 = CARTESIAN_POINT ( 'NONE',  ( -49.99999999999999289, 39.90000000000001279, -16.24598481164531449 ) ) ;
#5796 = CARTESIAN_POINT ( 'NONE',  ( -40.34137639590981195, 38.12187500034139731, 29.30972558990012189 ) ) ;
#5797 = PLANE ( 'NONE',  #1401 ) ;
#5798 = ORIENTED_EDGE ( 'NONE', *, *, #2349, .T. ) ;
#5799 = CARTESIAN_POINT ( 'NONE',  ( -49.86468353125000164, 39.92187500034139447, 0.000000000000000000 ) ) ;
#5800 = VERTEX_POINT ( 'NONE', #7290 ) ;
#5801 = EDGE_LOOP ( 'NONE', ( #5706, #10303, #2939, #5740 ) ) ;
#5802 = ADVANCED_FACE ( 'NONE', ( #1031 ), #4629, .T. ) ;
#5803 =( BOUNDED_CURVE ( )  B_SPLINE_CURVE ( 2, ( #10954, #13526, #3395, #1045, #16019, #3304, #16193, #7142, #7218, #8611, #4647, #7389, #9877 ),
 .UNSPECIFIED., .F., .F. ) 
 B_SPLINE_CURVE_WITH_KNOTS ( ( 3, 2, 2, 2, 2, 2, 3 ),
 ( 0.7500000000000000000, 0.7533333333333332993, 0.7600000000000000089, 0.7666666666666667185, 0.7733333333333333171, 0.7800000000000000266, 0.7833333333333333259 ),
 .UNSPECIFIED. ) 
 CURVE ( )  GEOMETRIC_REPRESENTATION_ITEM ( )  RATIONAL_B_SPLINE_CURVE ( ( 0.9755282581475768211, 0.9755282581475768211, 1.000000000000000000, 0.9510565162951535312, 1.000000000000000000, 0.9510565162951535312, 1.000000000000000000, 0.9510565162951535312, 1.000000000000000000, 0.9510565162951535312, 1.000000000000000000, 0.9755282581475768211, 0.9755282581475768211 ) ) 
 REPRESENTATION_ITEM ( '' )  );
#5804 = ORIENTED_EDGE ( 'NONE', *, *, #12255, .F. ) ;
#5805 = LINE ( 'NONE', #12276, #8378 ) ;
#5806 = CARTESIAN_POINT ( 'NONE',  ( 11.92169313911843354, 33.90715708214350599, 102.0000000000000142 ) ) ;
#5807 = DIRECTION ( 'NONE',  ( -1.000000000000000000, 0.000000000000000000, 0.000000000000000000 ) ) ;
#5808 = CARTESIAN_POINT ( 'NONE',  ( 7.919222016226758143, 36.33250428222963535, 50.00000000000000711 ) ) ;
#5809 = EDGE_CURVE ( 'NONE', #15952, #12012, #7375, .T. ) ;
#5810 = CARTESIAN_POINT ( 'NONE',  ( -40.34137639590981195, 38.05937500034139731, 29.30972558990012189 ) ) ;
#5811 = CARTESIAN_POINT ( 'NONE',  ( -16.50000000000000711, 22.50000000000000000, 102.0000000000000142 ) ) ;
#5812 = DIRECTION ( 'NONE',  ( -0.000000000000000000, -1.000000000000000000, -0.000000000000000000 ) ) ;
#5813 = EDGE_CURVE ( 'NONE', #58, #894, #7529, .T. ) ;
#5814 = LINE ( 'NONE', #808, #13967 ) ;
#5815 = CARTESIAN_POINT ( 'NONE',  ( -2.500000000000000000, 247.0000000000000284, 47.99999999999999289 ) ) ;
#5816 = FACE_OUTER_BOUND ( 'NONE', #9542, .T. ) ;
#5817 = EDGE_CURVE ( 'NONE', #12542, #16246, #2114, .T. ) ;
#5818 = CARTESIAN_POINT ( 'NONE',  ( 0.000000000000000000, 22.50000000000000000, 102.0000000000000142 ) ) ;
#5819 = B_SPLINE_CURVE_WITH_KNOTS ( 'NONE', 3,
 ( #11551, #15625, #7979, #8146 ),
 .UNSPECIFIED., .F., .F.,
 ( 4, 4 ),
 ( 2.829004760655812661E-07, 0.001414802801989366136 ),
 .UNSPECIFIED. ) ;
#5820 = CARTESIAN_POINT ( 'NONE',  ( 7.919222016226809657, 25.22999571913595318, -50.00000000000000000 ) ) ;
#5821 = EDGE_LOOP ( 'NONE', ( #14608, #3533, #535, #8328 ) ) ;
#5822 = CARTESIAN_POINT ( 'NONE',  ( -30.81806926056962226, 34.15937500034139163, 42.41743335407647919 ) ) ;
#5823 = ORIENTED_EDGE ( 'NONE', *, *, #3585, .T. ) ;
#5824 = ORIENTED_EDGE ( 'NONE', *, *, #8585, .F. ) ;
#5825 = ORIENTED_EDGE ( 'NONE', *, *, #11432, .T. ) ;
#5826 = CARTESIAN_POINT ( 'NONE',  ( -49.99999999999999289, 43.68125000068279462, -16.24598481164531449 ) ) ;
#5827 = STYLED_ITEM ( 'NONE', ( #7630 ), #3161 ) ;
#5828 = CARTESIAN_POINT ( 'NONE',  ( -1.514495797847258629, 99.85985911164404172, 9.657683769731226775 ) ) ;
#5829 = CARTESIAN_POINT ( 'NONE',  ( 30.90169943749473802, 29.30000000000000071, -42.53254041760200721 ) ) ;
#5830 = VERTEX_POINT ( 'NONE', #14744 ) ;
#5831 = CARTESIAN_POINT ( 'NONE',  ( 0.000000000000000000, 217.0000000000000284, 40.00000000000000000 ) ) ;
#5832 = FILL_AREA_STYLE ('',( #3500 ) ) ;
#5833 = CARTESIAN_POINT ( 'NONE',  ( -13.21840623068678866, 11.01752607032678455, 97.16300551537720764 ) ) ;
#5834 = CARTESIAN_POINT ( 'NONE',  ( 0.000000000000000000, 261.9999999999999432, 0.000000000000000000 ) ) ;
#5835 = LINE ( 'NONE', #8239, #3549 ) ;
#5836 = CYLINDRICAL_SURFACE ( 'NONE', #4503, 9.080892972013911546 ) ;
#5837 = LINE ( 'NONE', #12306, #680 ) ;
#5838 = CARTESIAN_POINT ( 'NONE',  ( 15.45084971874736723, 37.18125000068280173, -47.55282581475768211 ) ) ;
#5839 = CARTESIAN_POINT ( 'NONE',  ( -41.19975849074612029, 20.00000000000000355, 28.55207485309411553 ) ) ;
#5840 = EDGE_CURVE ( 'NONE', #5867, #16127, #8444, .T. ) ;
#5841 = CARTESIAN_POINT ( 'NONE',  ( -48.35726954556750457, 20.00000000000000355, 12.16803787670978387 ) ) ;
#5842 =( BOUNDED_SURFACE ( )  B_SPLINE_SURFACE ( 1, 2, ( 
 ( #6677, #8065, #11893, #4335, #2836, #10729, #11807, #5515, #14449, #247, #3074, #4177, #7904, #1585, #15790, #5428, #491, #11727, #9490, #13060, #327, #10654, #14536, #10487, #3162, #15545, #1505, #14297, #2920, #6762, #16207, #12219, #8310, #3494, #2147, #8233, #647, #15880, #8549, #983, #8391, #13463, #5910, #5744, #15956, #9732, #7072, #14613, #13376, #14695, #12138, #12048, #1980, #9893, #10818, #14781, #2070, #10892, #741, #4502, #12295, #5826, #4663, #3412, #16131, #9569, #6082, #7159, #821, #4758, #1898, #14866, #4577, #6991, #3237, #11149, #9641, #7235, #3321, #7320, #10970, #16036, #897, #8477, #13542, #13619, #5993, #14948, #2228, #11061, #9814, #4838, #12386, #13298, #15501, #14170, #3575, #12471, #11227, #4125, #13019, #3959, #9034, #1456, #1063, #11305, #5312, #2398, #9975, #8718, #10288, #7476, #7402, #13784, #5467, #6155, #10362, #10536, #16283, #14089, #2788, #5007, #15422, #2704, #10444, #5386, #15342, #7782, #12544, #8631, #207, #12853, #13701, #6551, #2318, #365, #1140, #11612, #6234, #12942, #2878, #9202, #4042, #1546, #4921, #16367, #14258, #15032, #9111, #7864, #3662, #6638, #11687, #287, #7946, #1621, #6715, #11765, #4543, #2030, #9606, #779, #15921, #1703, #12091, #11853, #3200, #8352, #6957, #14495, #533, #4374, #6880, #7121, #12179, #4464, #3124, #13185, #15839, #14654, #5788, #6799, #3282, #15673, #8196, #4296, #10855, #9530, #15595, #8022, #454, #13415, #5871, #15746, #9441, #13262, #13098, #11933, #609, #14410, #5555, #9360, #5628, #3033, #2955, #8103, #4216, #10617, #5705, #9284, #1789, #1862, #14576, #10690, #10772, #12011, #14338, #699, #8274, #13338, #1942, #7035, #7371, #940, #4623, #3537, #9686, #7518, #4720, #11112, #9778, #3622, #10028, #6199, #16171, #8685, #2109, #14825, #16329, #10933, #16081, #3455, #7196, #8516, #14736, #16247, #7447, #3707, #14908, #3370, #4966, #13828, #15080, #12590, #11271, #13501, #12512, #12259, #14992, #8766, #2275, #9856, #12341, #4803, #2187, #2440, #1186, #4880, #8591, #13581, #11194, #15996, #1104, #861, #8438, #11017, #13664, #7283, #6041, #5954, #13750, #12434, #1027, #6122, #2363, #9938, #15485, #5209, #10267, #14155, #16420, #12923, #13996, #5055, #10106, #4109, #15237, #191, #26, #5376, #1356 ),
 ( #6448, #14240, #8846, #2771, #2526, #10346, #9180, #14075, #15327, #7689, #11507, #2613, #2861, #7930, #11592, #3946, #3864, #6529, #11672, #1529, #13907, #271, #6368, #104, #8934, #5132, #3784, #15410, #10185, #2690, #7765, #7846, #7605, #13003, #9019, #12836, #6619, #15158, #10430, #12759, #12682, #1278, #6283, #1440, #5298, #4027, #11355, #9097, #11434, #10753, #10677, #15656, #1922, #5541, #3263, #12071, #2941, #13161, #9591, #5612, #1687, #13321, #11994, #1607, #10515, #9266, #7016, #10840, #1771, #6869, #15729, #15576, #9345, #3104, #438, #8008, #6784, #8088, #10601, #5450, #11829, #8333, #4202, #8179, #6700, #14322, #11919, #592, #3017, #13246, #517, #8257, #3184, #4359, #9423, #4281, #11750, #14471, #1845, #351, #6941, #13082, #14638, #14396, #5684, #15814, #4446, #673, #5771, #9512, #14560, #15904, #4527, #2344, #13397, #2092, #5936, #9665, #11000, #12161, #2252, #9920, #6179, #922, #5853, #7425, #16310, #12494, #15060, #13731, #13564, #4781, #4692, #3599, #16230, #4863, #7104, #9840, #11251, #763, #11089, #13643, #14973, #14891, #12320, #16060, #9760, #844, #3689, #14716, #4945, #14805, #7264, #3437, #2170, #8662, #1087, #6020, #7181, #10916, #10003, #2007, #7350, #15979, #4605, #12242, #3348, #8419, #13485, #8500, #1006, #16153, #3519, #12415, #8572, #6105, #11175, #11482, #11412, #12896, #6505, #249, #171, #15302, #5276, #12569, #7822, #13971, #10239, #13808, #10409, #10326, #1413, #1507, #15385, #11561, #1164, #5185, #4006, #9077, #14131, #2748, #4, #6599, #3924, #7498, #15134, #11652, #6261, #8996, #2591, #2500, #5032, #10160, #7743, #5354, #2420, #15464, #8743, #12811, #11333, #16398, #10085, #3762, #5106, #8821, #13885, #14054, #7577, #12659, #7666, #1254, #6346, #15212, #2670, #3841, #8906, #12736, #1332, #80, #6424, #11895, #3079, #5664, #1900, #4260, #5517, #2838, #14538, #2922, #13139, #9404, #8235, #6993, #8158, #10656, #3165, #9156, #13300, #14212, #9326, #494, #11809, #10732, #6920, #11973, #7906, #5594, #12050, #12983, #1746, #4338, #570, #15709, #2997, #6764, #412, #7988, #5749, #5430, #649, #10579, #14377, #15636, #8067, #15792, #4419, #6847, #14300, #1587, #10820, #4085, #14451, #6679, #11729, #13062, #330, #10489, #15548, #1665, #13225 ) ),
 .UNSPECIFIED., .F., .F., .F. ) 
 B_SPLINE_SURFACE_WITH_KNOTS ( ( 2, 2 ),
 ( 3, 2, 2, 2, 2, 2, 2, 2, 2, 2, 2, 2, 2, 2, 2, 2, 2, 2, 2, 2, 2, 2, 2, 2, 2, 2, 2, 2, 2, 2, 2, 2, 2, 2, 2, 2, 2, 2, 2, 2, 2, 2, 2, 2, 2, 2, 2, 2, 2, 2, 2, 2, 2, 2, 2, 2, 2, 2, 2, 2, 2, 2, 2, 2, 2, 2, 2, 2, 2, 2, 2, 2, 2, 2, 2, 2, 2, 2, 2, 2, 2, 2, 2, 2, 2, 2, 2, 2, 2, 2, 2, 2, 2, 2, 2, 2, 2, 2, 2, 2, 2, 2, 2, 2, 2, 2, 2, 2, 2, 2, 2, 2, 2, 2, 2, 2, 2, 2, 2, 2, 2, 2, 2, 2, 2, 2, 2, 2, 2, 2, 2, 2, 2, 2, 2, 2, 2, 2, 2, 2, 2, 2, 2, 2, 2, 2, 2, 2, 2, 2, 3 ),
 ( 0.000000000000000000, 1.000000000000000000 ),
 ( 0.000000000000000000, 0.006666666666666667095, 0.01333333333333333419, 0.02000000000000000042, 0.02666666666666666838, 0.03333333333333333287, 0.04000000000000000083, 0.04666666666666666879, 0.05333333333333333676, 0.05999999999999999778, 0.06666666666666666574, 0.07333333333333333370, 0.08000000000000000167, 0.08666666666666666963, 0.09333333333333333759, 0.1000000000000000056, 0.1066666666666666735, 0.1133333333333333276, 0.1199999999999999956, 0.1266666666666666774, 0.1333333333333333315, 0.1400000000000000133, 0.1466666666666666674, 0.1533333333333333215, 0.1600000000000000033, 0.1666666666666666574, 0.1733333333333333393, 0.1799999999999999933, 0.1866666666666666752, 0.1933333333333333293, 0.2000000000000000111, 0.2066666666666666652, 0.2133333333333333470, 0.2200000000000000011, 0.2266666666666666552, 0.2333333333333333370, 0.2399999999999999911, 0.2466666666666666730, 0.2533333333333333548, 0.2600000000000000089, 0.2666666666666666630, 0.2733333333333333171, 0.2800000000000000266, 0.2866666666666666807, 0.2933333333333333348, 0.2999999999999999889, 0.3066666666666666430, 0.3133333333333333526, 0.3200000000000000067, 0.3266666666666666607, 0.3333333333333333148, 0.3400000000000000244, 0.3466666666666666785, 0.3533333333333333326, 0.3599999999999999867, 0.3666666666666666408, 0.3733333333333333504, 0.3800000000000000044, 0.3866666666666666585, 0.3933333333333333126, 0.4000000000000000222, 0.4066666666666666763, 0.4133333333333333304, 0.4199999999999999845, 0.4266666666666666941, 0.4333333333333333481, 0.4400000000000000022, 0.4466666666666666563, 0.4533333333333333104, 0.4600000000000000200, 0.4666666666666666741, 0.4733333333333333282, 0.4799999999999999822, 0.4866666666666666918, 0.4933333333333333459, 0.5000000000000000000, 0.5066666666666667096, 0.5133333333333333082, 0.5200000000000000178, 0.5266666666666666163, 0.5333333333333333259, 0.5400000000000000355, 0.5466666666666666341, 0.5533333333333333437, 0.5600000000000000533, 0.5666666666666666519, 0.5733333333333333615, 0.5799999999999999600, 0.5866666666666666696, 0.5933333333333333792, 0.5999999999999999778, 0.6066666666666666874, 0.6133333333333332860, 0.6199999999999999956, 0.6266666666666667052, 0.6333333333333333037, 0.6400000000000000133, 0.6466666666666666119, 0.6533333333333333215, 0.6600000000000000311, 0.6666666666666666297, 0.6733333333333333393, 0.6800000000000000488, 0.6866666666666666474, 0.6933333333333333570, 0.6999999999999999556, 0.7066666666666666652, 0.7133333333333333748, 0.7199999999999999734, 0.7266666666666666829, 0.7333333333333332815, 0.7399999999999999911, 0.7466666666666667007, 0.7533333333333332993, 0.7600000000000000089, 0.7666666666666667185, 0.7733333333333333171, 0.7800000000000000266, 0.7866666666666666252, 0.7933333333333333348, 0.8000000000000000444, 0.8066666666666666430, 0.8133333333333333526, 0.8199999999999999512, 0.8266666666666666607, 0.8333333333333333703, 0.8399999999999999689, 0.8466666666666666785, 0.8533333333333333881, 0.8599999999999999867, 0.8666666666666666963, 0.8733333333333332948, 0.8800000000000000044, 0.8866666666666667140, 0.8933333333333333126, 0.9000000000000000222, 0.9066666666666666208, 0.9133333333333333304, 0.9200000000000000400, 0.9266666666666666385, 0.9333333333333333481, 0.9399999999999999467, 0.9466666666666666563, 0.9533333333333333659, 0.9599999999999999645, 0.9666666666666666741, 0.9733333333333333837, 0.9799999999999999822, 0.9866666666666666918, 0.9933333333333332904, 1.000000000000000000 ),
 .UNSPECIFIED. ) 
 GEOMETRIC_REPRESENTATION_ITEM ( )  RATIONAL_B_SPLINE_SURFACE ( (
 ( 1.000000000000000000, 0.9510565162951535312, 1.000000000000000000, 0.9510565162951535312, 1.000000000000000000, 0.9510565162951535312, 1.000000000000000000, 0.9510565162951535312, 1.000000000000000000, 0.9510565162951535312, 1.000000000000000000, 0.9510565162951535312, 1.000000000000000000, 0.9510565162951535312, 1.000000000000000000, 0.9510565162951535312, 1.000000000000000000, 0.9510565162951535312, 1.000000000000000000, 0.9510565162951535312, 1.000000000000000000, 0.9510565162951535312, 1.000000000000000000, 0.9510565162951535312, 1.000000000000000000, 0.9510565162951535312, 1.000000000000000000, 0.9510565162951535312, 1.000000000000000000, 0.9510565162951535312, 1.000000000000000000, 0.9510565162951535312, 1.000000000000000000, 0.9510565162951535312, 1.000000000000000000, 0.9510565162951535312, 1.000000000000000000, 0.9510565162951535312, 1.000000000000000000, 0.9510565162951535312, 1.000000000000000000, 0.9510565162951535312, 1.000000000000000000, 0.9510565162951535312, 1.000000000000000000, 0.9510565162951535312, 1.000000000000000000, 0.9510565162951535312, 1.000000000000000000, 0.9510565162951535312, 1.000000000000000000, 0.9510565162951535312, 1.000000000000000000, 0.9510565162951535312, 1.000000000000000000, 0.9510565162951535312, 1.000000000000000000, 0.9510565162951535312, 1.000000000000000000, 0.9510565162951535312, 1.000000000000000000, 0.9510565162951535312, 1.000000000000000000, 0.9510565162951535312, 1.000000000000000000, 0.9510565162951535312, 1.000000000000000000, 0.9510565162951535312, 1.000000000000000000, 0.9510565162951535312, 1.000000000000000000, 0.9510565162951535312, 1.000000000000000000, 0.9510565162951535312, 1.000000000000000000, 0.9510565162951535312, 1.000000000000000000, 0.9510565162951535312, 1.000000000000000000, 0.9510565162951535312, 1.000000000000000000, 0.9510565162951535312, 1.000000000000000000, 0.9510565162951535312, 1.000000000000000000, 0.9510565162951535312, 1.000000000000000000, 0.9510565162951535312, 1.000000000000000000, 0.9510565162951535312, 1.000000000000000000, 0.9510565162951535312, 1.000000000000000000, 0.9510565162951535312, 1.000000000000000000, 0.9510565162951535312, 1.000000000000000000, 0.9510565162951535312, 1.000000000000000000, 0.9510565162951535312, 1.000000000000000000, 0.9510565162951535312, 1.000000000000000000, 0.9510565162951535312, 1.000000000000000000, 0.9510565162951535312, 1.000000000000000000, 0.9510565162951535312, 1.000000000000000000, 0.9510565162951535312, 1.000000000000000000, 0.9510565162951535312, 1.000000000000000000, 0.9510565162951535312, 1.000000000000000000, 0.9510565162951535312, 1.000000000000000000, 0.9510565162951535312, 1.000000000000000000, 0.9510565162951535312, 1.000000000000000000, 0.9510565162951535312, 1.000000000000000000, 0.9510565162951535312, 1.000000000000000000, 0.9510565162951535312, 1.000000000000000000, 0.9510565162951535312, 1.000000000000000000, 0.9510565162951535312, 1.000000000000000000, 0.9510565162951535312, 1.000000000000000000, 0.9510565162951535312, 1.000000000000000000, 0.9510565162951535312, 1.000000000000000000, 0.9510565162951535312, 1.000000000000000000, 0.9510565162951535312, 1.000000000000000000, 0.9510565162951535312, 1.000000000000000000, 0.9510565162951535312, 1.000000000000000000, 0.9510565162951535312, 1.000000000000000000, 0.9510565162951535312, 1.000000000000000000, 0.9510565162951535312, 1.000000000000000000, 0.9510565162951535312, 1.000000000000000000, 0.9510565162951535312, 1.000000000000000000, 0.9510565162951535312, 1.000000000000000000, 0.9510565162951535312, 1.000000000000000000, 0.9510565162951535312, 1.000000000000000000, 0.9510565162951535312, 1.000000000000000000, 0.9510565162951535312, 1.000000000000000000, 0.9510565162951535312, 1.000000000000000000, 0.9510565162951535312, 1.000000000000000000, 0.9510565162951535312, 1.000000000000000000, 0.9510565162951535312, 1.000000000000000000, 0.9510565162951535312, 1.000000000000000000, 0.9510565162951535312, 1.000000000000000000, 0.9510565162951535312, 1.000000000000000000, 0.9510565162951535312, 1.000000000000000000, 0.9510565162951535312, 1.000000000000000000, 0.9510565162951535312, 1.000000000000000000, 0.9510565162951535312, 1.000000000000000000, 0.9510565162951535312, 1.000000000000000000, 0.9510565162951535312, 1.000000000000000000, 0.9510565162951535312, 1.000000000000000000, 0.9510565162951535312, 1.000000000000000000, 0.9510565162951535312, 1.000000000000000000, 0.9510565162951535312, 1.000000000000000000, 0.9510565162951535312, 1.000000000000000000, 0.9510565162951535312, 1.000000000000000000, 0.9510565162951535312, 1.000000000000000000, 0.9510565162951535312, 1.000000000000000000, 0.9510565162951535312, 1.000000000000000000, 0.9510565162951535312, 1.000000000000000000, 0.9510565162951535312, 1.000000000000000000, 0.9510565162951535312, 1.000000000000000000, 0.9510565162951535312, 1.000000000000000000, 0.9510565162951535312, 1.000000000000000000, 0.9510565162951535312, 1.000000000000000000, 0.9510565162951535312, 1.000000000000000000, 0.9510565162951535312, 1.000000000000000000, 0.9510565162951535312, 1.000000000000000000, 0.9510565162951535312, 1.000000000000000000, 0.9510565162951535312, 1.000000000000000000, 0.9510565162951535312, 1.000000000000000000, 0.9510565162951535312, 1.000000000000000000, 0.9510565162951535312, 1.000000000000000000, 0.9510565162951535312, 1.000000000000000000, 0.9510565162951535312, 1.000000000000000000, 0.9510565162951535312, 1.000000000000000000, 0.9510565162951535312, 1.000000000000000000, 0.9510565162951535312, 1.000000000000000000, 0.9510565162951535312, 1.000000000000000000, 0.9510565162951535312, 1.000000000000000000, 0.9510565162951535312, 1.000000000000000000, 0.9510565162951535312, 1.000000000000000000, 0.9510565162951535312, 1.000000000000000000, 0.9510565162951535312, 1.000000000000000000, 0.9510565162951535312, 1.000000000000000000, 0.9510565162951535312, 1.000000000000000000, 0.9510565162951535312, 1.000000000000000000, 0.9510565162951535312, 1.000000000000000000, 0.9510565162951535312, 1.000000000000000000, 0.9510565162951535312, 1.000000000000000000, 0.9510565162951535312, 1.000000000000000000, 0.9510565162951535312, 1.000000000000000000, 0.9510565162951535312, 1.000000000000000000, 0.9510565162951535312, 1.000000000000000000, 0.9510565162951535312, 1.000000000000000000, 0.9510565162951535312, 1.000000000000000000, 0.9510565162951535312, 1.000000000000000000, 0.9510565162951535312, 1.000000000000000000, 0.9510565162951535312, 1.000000000000000000, 0.9510565162951535312, 1.000000000000000000, 0.9510565162951535312, 1.000000000000000000, 0.9510565162951535312, 1.000000000000000000, 0.9510565162951535312, 1.000000000000000000, 0.9510565162951535312, 1.000000000000000000, 0.9510565162951535312, 1.000000000000000000),
 ( 1.000000000000000000, 0.9510565162951535312, 1.000000000000000000, 0.9510565162951535312, 1.000000000000000000, 0.9510565162951535312, 1.000000000000000000, 0.9510565162951535312, 1.000000000000000000, 0.9510565162951535312, 1.000000000000000000, 0.9510565162951535312, 1.000000000000000000, 0.9510565162951535312, 1.000000000000000000, 0.9510565162951535312, 1.000000000000000000, 0.9510565162951535312, 1.000000000000000000, 0.9510565162951535312, 1.000000000000000000, 0.9510565162951535312, 1.000000000000000000, 0.9510565162951535312, 1.000000000000000000, 0.9510565162951535312, 1.000000000000000000, 0.9510565162951535312, 1.000000000000000000, 0.9510565162951535312, 1.000000000000000000, 0.9510565162951535312, 1.000000000000000000, 0.9510565162951535312, 1.000000000000000000, 0.9510565162951535312, 1.000000000000000000, 0.9510565162951535312, 1.000000000000000000, 0.9510565162951535312, 1.000000000000000000, 0.9510565162951535312, 1.000000000000000000, 0.9510565162951535312, 1.000000000000000000, 0.9510565162951535312, 1.000000000000000000, 0.9510565162951535312, 1.000000000000000000, 0.9510565162951535312, 1.000000000000000000, 0.9510565162951535312, 1.000000000000000000, 0.9510565162951535312, 1.000000000000000000, 0.9510565162951535312, 1.000000000000000000, 0.9510565162951535312, 1.000000000000000000, 0.9510565162951535312, 1.000000000000000000, 0.9510565162951535312, 1.000000000000000000, 0.9510565162951535312, 1.000000000000000000, 0.9510565162951535312, 1.000000000000000000, 0.9510565162951535312, 1.000000000000000000, 0.9510565162951535312, 1.000000000000000000, 0.9510565162951535312, 1.000000000000000000, 0.9510565162951535312, 1.000000000000000000, 0.9510565162951535312, 1.000000000000000000, 0.9510565162951535312, 1.000000000000000000, 0.9510565162951535312, 1.000000000000000000, 0.9510565162951535312, 1.000000000000000000, 0.9510565162951535312, 1.000000000000000000, 0.9510565162951535312, 1.000000000000000000, 0.9510565162951535312, 1.000000000000000000, 0.9510565162951535312, 1.000000000000000000, 0.9510565162951535312, 1.000000000000000000, 0.9510565162951535312, 1.000000000000000000, 0.9510565162951535312, 1.000000000000000000, 0.9510565162951535312, 1.000000000000000000, 0.9510565162951535312, 1.000000000000000000, 0.9510565162951535312, 1.000000000000000000, 0.9510565162951535312, 1.000000000000000000, 0.9510565162951535312, 1.000000000000000000, 0.9510565162951535312, 1.000000000000000000, 0.9510565162951535312, 1.000000000000000000, 0.9510565162951535312, 1.000000000000000000, 0.9510565162951535312, 1.000000000000000000, 0.9510565162951535312, 1.000000000000000000, 0.9510565162951535312, 1.000000000000000000, 0.9510565162951535312, 1.000000000000000000, 0.9510565162951535312, 1.000000000000000000, 0.9510565162951535312, 1.000000000000000000, 0.9510565162951535312, 1.000000000000000000, 0.9510565162951535312, 1.000000000000000000, 0.9510565162951535312, 1.000000000000000000, 0.9510565162951535312, 1.000000000000000000, 0.9510565162951535312, 1.000000000000000000, 0.9510565162951535312, 1.000000000000000000, 0.9510565162951535312, 1.000000000000000000, 0.9510565162951535312, 1.000000000000000000, 0.9510565162951535312, 1.000000000000000000, 0.9510565162951535312, 1.000000000000000000, 0.9510565162951535312, 1.000000000000000000, 0.9510565162951535312, 1.000000000000000000, 0.9510565162951535312, 1.000000000000000000, 0.9510565162951535312, 1.000000000000000000, 0.9510565162951535312, 1.000000000000000000, 0.9510565162951535312, 1.000000000000000000, 0.9510565162951535312, 1.000000000000000000, 0.9510565162951535312, 1.000000000000000000, 0.9510565162951535312, 1.000000000000000000, 0.9510565162951535312, 1.000000000000000000, 0.9510565162951535312, 1.000000000000000000, 0.9510565162951535312, 1.000000000000000000, 0.9510565162951535312, 1.000000000000000000, 0.9510565162951535312, 1.000000000000000000, 0.9510565162951535312, 1.000000000000000000, 0.9510565162951535312, 1.000000000000000000, 0.9510565162951535312, 1.000000000000000000, 0.9510565162951535312, 1.000000000000000000, 0.9510565162951535312, 1.000000000000000000, 0.9510565162951535312, 1.000000000000000000, 0.9510565162951535312, 1.000000000000000000, 0.9510565162951535312, 1.000000000000000000, 0.9510565162951535312, 1.000000000000000000, 0.9510565162951535312, 1.000000000000000000, 0.9510565162951535312, 1.000000000000000000, 0.9510565162951535312, 1.000000000000000000, 0.9510565162951535312, 1.000000000000000000, 0.9510565162951535312, 1.000000000000000000, 0.9510565162951535312, 1.000000000000000000, 0.9510565162951535312, 1.000000000000000000, 0.9510565162951535312, 1.000000000000000000, 0.9510565162951535312, 1.000000000000000000, 0.9510565162951535312, 1.000000000000000000, 0.9510565162951535312, 1.000000000000000000, 0.9510565162951535312, 1.000000000000000000, 0.9510565162951535312, 1.000000000000000000, 0.9510565162951535312, 1.000000000000000000, 0.9510565162951535312, 1.000000000000000000, 0.9510565162951535312, 1.000000000000000000, 0.9510565162951535312, 1.000000000000000000, 0.9510565162951535312, 1.000000000000000000, 0.9510565162951535312, 1.000000000000000000, 0.9510565162951535312, 1.000000000000000000, 0.9510565162951535312, 1.000000000000000000, 0.9510565162951535312, 1.000000000000000000, 0.9510565162951535312, 1.000000000000000000, 0.9510565162951535312, 1.000000000000000000, 0.9510565162951535312, 1.000000000000000000, 0.9510565162951535312, 1.000000000000000000, 0.9510565162951535312, 1.000000000000000000, 0.9510565162951535312, 1.000000000000000000, 0.9510565162951535312, 1.000000000000000000, 0.9510565162951535312, 1.000000000000000000, 0.9510565162951535312, 1.000000000000000000, 0.9510565162951535312, 1.000000000000000000, 0.9510565162951535312, 1.000000000000000000, 0.9510565162951535312, 1.000000000000000000, 0.9510565162951535312, 1.000000000000000000, 0.9510565162951535312, 1.000000000000000000, 0.9510565162951535312, 1.000000000000000000, 0.9510565162951535312, 1.000000000000000000, 0.9510565162951535312, 1.000000000000000000, 0.9510565162951535312, 1.000000000000000000, 0.9510565162951535312, 1.000000000000000000, 0.9510565162951535312, 1.000000000000000000, 0.9510565162951535312, 1.000000000000000000, 0.9510565162951535312, 1.000000000000000000, 0.9510565162951535312, 1.000000000000000000, 0.9510565162951535312, 1.000000000000000000, 0.9510565162951535312, 1.000000000000000000, 0.9510565162951535312, 1.000000000000000000, 0.9510565162951535312, 1.000000000000000000, 0.9510565162951535312, 1.000000000000000000, 0.9510565162951535312, 1.000000000000000000, 0.9510565162951535312, 1.000000000000000000, 0.9510565162951535312, 1.000000000000000000, 0.9510565162951535312, 1.000000000000000000, 0.9510565162951535312, 1.000000000000000000) ) ) 
 REPRESENTATION_ITEM ( '' )  SURFACE ( )  );
#5843 = DIRECTION ( 'NONE',  ( -1.156482317317871478E-16, 0.000000000000000000, -1.000000000000000000 ) ) ;
#5844 = AXIS2_PLACEMENT_3D ( 'NONE', #10225, #15277, #5012 ) ;
#5845 = CARTESIAN_POINT ( 'NONE',  ( 30.90169943749474157, 31.30000000000000071, -42.53254041760200721 ) ) ;
#5846 = CARTESIAN_POINT ( 'NONE',  ( 15.40903463028482356, 26.45937500034139589, 47.42413220539093999 ) ) ;
#5847 = EDGE_CURVE ( 'NONE', #11087, #9397, #9038, .T. ) ;
#5848 = CARTESIAN_POINT ( 'NONE',  ( -15.45084971874737256, 29.60000000000000142, -47.55282581475767500 ) ) ;
#5849 = ORIENTED_EDGE ( 'NONE', *, *, #3392, .T. ) ;
#5850 = B_SPLINE_CURVE_WITH_KNOTS ( 'NONE', 3,
 ( #11310, #8636, #62, #13709 ),
 .UNSPECIFIED., .F., .F.,
 ( 4, 4 ),
 ( 2.829004760671193191E-07, 0.001414802801989366787 ),
 .UNSPECIFIED. ) ;
#5851 = ORIENTED_EDGE ( 'NONE', *, *, #13222, .F. ) ;
#5852 = DIRECTION ( 'NONE',  ( 0.4999999999999918954, 0.8660254037844433705, 0.000000000000000000 ) ) ;
#5853 = CARTESIAN_POINT ( 'NONE',  ( -15.40903463028481646, 37.45937500034139589, -47.42413220539093999 ) ) ;
#5854 = CARTESIAN_POINT ( 'NONE',  ( 7.919222016226822092, 48.33250428222964246, 49.99999999999999289 ) ) ;
#5855 = DIRECTION ( 'NONE',  ( -0.8660254037844361541, 0.000000000000000000, 0.5000000000000042188 ) ) ;
#5856 = CARTESIAN_POINT ( 'NONE',  ( 15.45084971874736723, 45.18125000068280173, -47.55282581475768211 ) ) ;
#5857 = CARTESIAN_POINT ( 'NONE',  ( 49.86468353124999453, 31.02187500034139234, -16.20201782572376459 ) ) ;
#5858 = CARTESIAN_POINT ( 'NONE',  ( 49.86468353125001585, 26.75937500034139660, 16.20201782572375038 ) ) ;
#5859 = DIRECTION ( 'NONE',  ( 0.000000000000000000, 0.000000000000000000, 1.000000000000000000 ) ) ;
#5860 = CARTESIAN_POINT ( 'NONE',  ( 15.40903463028481113, 31.32187500034139305, -47.42413220539094709 ) ) ;
#5861 = DIRECTION ( 'NONE',  ( 0.000000000000000000, 0.7071067811865463515, -0.7071067811865487940 ) ) ;
#5862 = CARTESIAN_POINT ( 'NONE',  ( -49.86468353125000164, 45.85937500034140157, 0.000000000000000000 ) ) ;
#5863 = CARTESIAN_POINT ( 'NONE',  ( -40.34137639590981195, 38.12187500034139731, 29.30972558990012189 ) ) ;
#5864 = EDGE_CURVE ( 'NONE', #10042, #5006, #12390, .T. ) ;
#5865 = CARTESIAN_POINT ( 'NONE',  ( 49.86468353124999453, 23.02187500034139944, -16.20201782572376459 ) ) ;
#5866 = EDGE_CURVE ( 'NONE', #8473, #11298, #1537, .T. ) ;
#5867 = VERTEX_POINT ( 'NONE', #6535 ) ;
#5868 = B_SPLINE_CURVE_WITH_KNOTS ( 'NONE', 3,
 ( #12052, #652, #15794, #1903 ),
 .UNSPECIFIED., .F., .F.,
 ( 4, 4 ),
 ( 2.829004760683457170E-07, 0.001414802801989366570 ),
 .UNSPECIFIED. ) ;
#5869 = CARTESIAN_POINT ( 'NONE',  ( 30.81806926056964002, 42.55937500034139020, 42.41743335407646498 ) ) ;
#5870 = VERTEX_POINT ( 'NONE', #5137 ) ;
#5871 = CARTESIAN_POINT ( 'NONE',  ( 40.45084971874737789, 30.58125000068279675, 29.38926261462365375 ) ) ;
#5872 = ORIENTED_EDGE ( 'NONE', *, *, #14727, .F. ) ;
#5873 = CARTESIAN_POINT ( 'NONE',  ( 2.600676159226420495E-13, 33.28125000068279604, -49.99999999999999289 ) ) ;
#5874 = CARTESIAN_POINT ( 'NONE',  ( 9.631387414534489405E-15, 42.42187500034140157, 52.43083105670540789 ) ) ;
#5875 = CARTESIAN_POINT ( 'NONE',  ( -40.34137639590981905, 47.72187500034139873, -29.30972558990011478 ) ) ;
#5876 = CARTESIAN_POINT ( 'NONE',  ( 1.486087262401875941, 13.10364194761998213, 101.0000000000000000 ) ) ;
#5877 = CARTESIAN_POINT ( 'NONE',  ( 49.86468353125001585, 22.82187500034138949, 16.20201782572375038 ) ) ;
#5878 = SHAPE_DEFINITION_REPRESENTATION ( #15551, #13393 ) ;
#5879 = CARTESIAN_POINT ( 'NONE',  ( 40.45084971874737789, 32.58125000068280031, 29.38926261462365375 ) ) ;
#5880 = CARTESIAN_POINT ( 'NONE',  ( -49.99999999999999289, 35.90000000000000568, -16.24598481164531449 ) ) ;
#5881 = CARTESIAN_POINT ( 'NONE',  ( -40.34137639590981195, 42.12187500034139731, 29.30972558990012189 ) ) ;
#5882 = CARTESIAN_POINT ( 'NONE',  ( 0.5000000000000009992, 31.99999999999998579, 101.0000000000000000 ) ) ;
#5883 = EDGE_LOOP ( 'NONE', ( #15156, #12547, #226, #11648, #1501, #3660, #7036, #10674, #10133, #1843, #8414, #15031, #8396 ) ) ;
#5884 = CARTESIAN_POINT ( 'NONE',  ( 49.86468353125000164, 44.92187500034140157, -6.106662507704105588E-15 ) ) ;
#5885 = CARTESIAN_POINT ( 'NONE',  ( 7.513064459987437071E-14, 42.28125000068280315, 50.00000000000000000 ) ) ;
#5886 = EDGE_LOOP ( 'NONE', ( #10870, #11725, #2073 ) ) ;
#5887 = ORIENTED_EDGE ( 'NONE', *, *, #3030, .F. ) ;
#5888 = ORIENTED_EDGE ( 'NONE', *, *, #5959, .F. ) ;
#5889 = CARTESIAN_POINT ( 'NONE',  ( -4.320770838041405604, 30.97531352606679178, 101.0000000000000000 ) ) ;
#5890 = FACE_OUTER_BOUND ( 'NONE', #13861, .T. ) ;
#5891 = CARTESIAN_POINT ( 'NONE',  ( -15.45084971874737256, 21.38125000068279746, -47.55282581475767500 ) ) ;
#5892 = DIRECTION ( 'NONE',  ( -0.9945218953682744001, 0.1045284632676435066, 0.000000000000000000 ) ) ;
#5893 = CARTESIAN_POINT ( 'NONE',  ( 15.40903463028481113, 39.25937500034140015, -47.42413220539094709 ) ) ;
#5894 = CARTESIAN_POINT ( 'NONE',  ( -2.464234863135557063, 13.31155363843772932, 102.0000000000000142 ) ) ;
#5895 = CARTESIAN_POINT ( 'NONE',  ( 15.45084971874736723, 25.40000000000000213, -47.55282581475768211 ) ) ;
#5896 = DIRECTION ( 'NONE',  ( -0.4999999999999918399, 0.000000000000000000, 0.8660254037844433705 ) ) ;
#5897 =( NAMED_UNIT ( * ) SI_UNIT ( $, .STERADIAN. ) SOLID_ANGLE_UNIT ( ) );
#5898 = CARTESIAN_POINT ( 'NONE',  ( 0.000000000000000000, 20.00000000000000355, 50.00000000000000000 ) ) ;
#5899 = CARTESIAN_POINT ( 'NONE',  ( 17.35186893731097868, 20.17349094513210161, 101.0000000000000000 ) ) ;
#5900 = EDGE_CURVE ( 'NONE', #14296, #12805, #15927, .T. ) ;
#5901 = EDGE_CURVE ( 'NONE', #3842, #5010, #6297, .T. ) ;
#5902 = CARTESIAN_POINT ( 'NONE',  ( 15.45084971874737789, 42.38125000068279746, 47.55282581475767500 ) ) ;
#5903 = CARTESIAN_POINT ( 'NONE',  ( 15.45084971874737789, 36.60000000000000142, 47.55282581475767500 ) ) ;
#5904 = ORIENTED_EDGE ( 'NONE', *, *, #10739, .T. ) ;
#5905 = CARTESIAN_POINT ( 'NONE',  ( -40.34137639590981905, 33.65937500034139873, -29.30972558990011478 ) ) ;
#5906 = EDGE_LOOP ( 'NONE', ( #8289, #10871, #10080, #3879 ) ) ;
#5907 = ORIENTED_EDGE ( 'NONE', *, *, #7051, .F. ) ;
#5908 = VERTEX_POINT ( 'NONE', #7772 ) ;
#5909 = EDGE_CURVE ( 'NONE', #8741, #12025, #11601, .T. ) ;
#5910 = CARTESIAN_POINT ( 'NONE',  ( -40.45084971874737789, 45.58125000068280031, -29.38926261462365730 ) ) ;
#5911 = DIRECTION ( 'NONE',  ( -0.03463303435789952950, -0.9463120918278121740, 0.3213938048432717909 ) ) ;
#5912 = CARTESIAN_POINT ( 'NONE',  ( 0.000000000000000000, 22.50000000000000000, 101.0000000000000000 ) ) ;
#5913 = ORIENTED_EDGE ( 'NONE', *, *, #13293, .F. ) ;
#5914 = DIRECTION ( 'NONE',  ( 0.000000000000000000, 0.000000000000000000, 1.000000000000000000 ) ) ;
#5915 = DIRECTION ( 'NONE',  ( 0.000000000000000000, 0.000000000000000000, -1.000000000000000000 ) ) ;
#5916 = EDGE_CURVE ( 'NONE', #13296, #9545, #277, .T. ) ;
#5917 = CARTESIAN_POINT ( 'NONE',  ( -4.611208113858000779, 5.578466101304616842, 98.91552298129929000 ) ) ;
#5918 = LINE ( 'NONE', #10978, #2019 ) ;
#5919 = DIRECTION ( 'NONE',  ( 0.000000000000000000, 0.000000000000000000, -1.000000000000000000 ) ) ;
#5920 = DIRECTION ( 'NONE',  ( 0.000000000000000000, 1.541976423090494894E-16, 1.000000000000000000 ) ) ;
#5922 = CARTESIAN_POINT ( 'NONE',  ( 1.293669679204937499E-13, 39.50000000000000711, -50.00000000000000000 ) ) ;
#5921 = VECTOR ( 'NONE', #1580, 1000.000000000000000 ) ;
#5923 = LINE ( 'NONE', #14624, #11510 ) ;
#5924 = CARTESIAN_POINT ( 'NONE',  ( -50.00000000000000000, 42.00000000000000000, 0.000000000000000000 ) ) ;
#5925 = CARTESIAN_POINT ( 'NONE',  ( 49.86468353125000164, 22.92187500034139802, -6.106662507704105588E-15 ) ) ;
#5926 = FACE_OUTER_BOUND ( 'NONE', #16365, .T. ) ;
#5927 = EDGE_CURVE ( 'NONE', #2250, #10795, #10192, .T. ) ;
#5928 = CARTESIAN_POINT ( 'NONE',  ( 30.90169943749474157, 25.30000000000000071, -42.53254041760200721 ) ) ;
#5929 = CARTESIAN_POINT ( 'NONE',  ( -49.86468353124999453, 27.75937500034139660, -16.20201782572375393 ) ) ;
#5930 = CARTESIAN_POINT ( 'NONE',  ( -40.45084971874737079, 30.20000000000000284, 29.38926261462367151 ) ) ;
#5931 = VERTEX_POINT ( 'NONE', #5304 ) ;
#5932 = VECTOR ( 'NONE', #16339, 1000.000000000000000 ) ;
#5933 = CARTESIAN_POINT ( 'NONE',  ( -3.210462471511496205E-15, 25.35937500034139802, -52.43083105670540789 ) ) ;
#5934 = ORIENTED_EDGE ( 'NONE', *, *, #3167, .F. ) ;
#5935 = DIRECTION ( 'NONE',  ( -0.000000000000000000, 1.000000000000000000, -0.000000000000000000 ) ) ;
#5936 = CARTESIAN_POINT ( 'NONE',  ( -15.40903463028480580, 38.25937500034140015, 47.42413220539094709 ) ) ;
#5937 = CARTESIAN_POINT ( 'NONE',  ( -1.240322475938754499E-13, 40.28125000068280315, 50.00000000000000000 ) ) ;
#5938 = DIRECTION ( 'NONE',  ( -1.000000000000000000, 0.000000000000000000, 1.734723475976807094E-17 ) ) ;
#5939 =( BOUNDED_CURVE ( )  B_SPLINE_CURVE ( 2, ( #2414, #4684, #3432, #7419, #11081, #16390, #4855, #16054, #14883, #8566, #7256, #13636, #12488 ),
 .UNSPECIFIED., .F., .F. ) 
 B_SPLINE_CURVE_WITH_KNOTS ( ( 3, 2, 2, 2, 2, 2, 3 ),
 ( 0.2500000000000000000, 0.2533333333333333548, 0.2600000000000000089, 0.2666666666666666630, 0.2733333333333333171, 0.2800000000000000266, 0.2833333333333333814 ),
 .UNSPECIFIED. ) 
 CURVE ( )  GEOMETRIC_REPRESENTATION_ITEM ( )  RATIONAL_B_SPLINE_CURVE ( ( 0.9755282581475765991, 0.9755282581475765991, 1.000000000000000000, 0.9510565162951535312, 1.000000000000000000, 0.9510565162951535312, 1.000000000000000000, 0.9510565162951535312, 1.000000000000000000, 0.9510565162951535312, 1.000000000000000000, 0.9755282581475765991, 0.9755282581475768211 ) ) 
 REPRESENTATION_ITEM ( '' )  );
#5940 = DIRECTION ( 'NONE',  ( -6.938893903907231459E-18, 1.000000000000000000, 5.551115123125782702E-17 ) ) ;
#5941 = CARTESIAN_POINT ( 'NONE',  ( -15.40903463028480580, 30.32187500034140015, 47.42413220539094709 ) ) ;
#5942 = CARTESIAN_POINT ( 'NONE',  ( -40.34137639590981195, 32.05937500034139731, 29.30972558990012189 ) ) ;
#5943 = CARTESIAN_POINT ( 'NONE',  ( 0.000000000000000000, 262.0000000000000000, 0.000000000000000000 ) ) ;
#5944 = CARTESIAN_POINT ( 'NONE',  ( -3.210462471511496205E-15, 33.42187500034140157, -52.43083105670540789 ) ) ;
#5945 = EDGE_CURVE ( 'NONE', #13541, #589, #6198, .T. ) ;
#5946 = CARTESIAN_POINT ( 'NONE',  ( 40.45084971874737079, 33.20000000000000284, -29.38926261462366440 ) ) ;
#5947 = CIRCLE ( 'NONE', #13099, 45.00000000000000711 ) ;
#5948 = CARTESIAN_POINT ( 'NONE',  ( 49.86468353125001585, 44.75937500034138594, 16.20201782572375038 ) ) ;
#5949 = CARTESIAN_POINT ( 'NONE',  ( 15.40903463028481113, 39.32187500034140015, -47.42413220539094709 ) ) ;
#5950 = CARTESIAN_POINT ( 'NONE',  ( -49.86468353125000164, 23.92187500034139447, 0.000000000000000000 ) ) ;
#5951 = VERTEX_POINT ( 'NONE', #5381 ) ;
#5952 = CARTESIAN_POINT ( 'NONE',  ( 15.40903463028482356, 44.45937500034139589, 47.42413220539093999 ) ) ;
#5953 = ORIENTED_EDGE ( 'NONE', *, *, #7386, .T. ) ;
#5954 = CARTESIAN_POINT ( 'NONE',  ( -49.99999999999999289, 21.88125000068280102, 16.24598481164533226 ) ) ;
#5955 = TOROIDAL_SURFACE ( 'NONE', #3020, 63.16733765196516970, 2.000000000000000000 ) ;
#5956 = ORIENTED_EDGE ( 'NONE', *, *, #3807, .F. ) ;
#5957 = CARTESIAN_POINT ( 'NONE',  ( 50.00000000000000000, 40.78125000068279604, -6.123233995736766085E-15 ) ) ;
#5958 = CARTESIAN_POINT ( 'NONE',  ( 30.81806926056962936, 39.22187500034139873, -42.41743335407646498 ) ) ;
#5959 = EDGE_CURVE ( 'NONE', #8386, #6499, #10353, .T. ) ;
#5960 = CARTESIAN_POINT ( 'NONE',  ( -30.81806926056963292, 49.62187500034139020, -42.41743335407647209 ) ) ;
#5961 = CARTESIAN_POINT ( 'NONE',  ( -49.86468353125000164, 21.92187500034139802, 0.000000000000000000 ) ) ;
#5962 = CONTEXT_DEPENDENT_SHAPE_REPRESENTATION ( #8982, #6539 ) ;
#5963 = CARTESIAN_POINT ( 'NONE',  ( -50.00000000000000000, 31.78125000068279959, 0.000000000000000000 ) ) ;
#5964 = CIRCLE ( 'NONE', #9151, 14.08089297201391155 ) ;
#5965 = CARTESIAN_POINT ( 'NONE',  ( -40.34137639590981195, 40.12187500034139731, 29.30972558990012189 ) ) ;
#5966 = CARTESIAN_POINT ( 'NONE',  ( -21.32168401022832782, 284.4942466288908918, -8.160842005118960074 ) ) ;
#5967 = EDGE_LOOP ( 'NONE', ( #3123, #4918 ) ) ;
#5968 = CARTESIAN_POINT ( 'NONE',  ( 9.631387414534489405E-15, 34.42187500034138736, 52.43083105670540789 ) ) ;
#5969 = VERTEX_POINT ( 'NONE', #6291 ) ;
#5970 = ORIENTED_EDGE ( 'NONE', *, *, #5416, .T. ) ;
#5971 = ORIENTED_EDGE ( 'NONE', *, *, #8026, .T. ) ;
#5972 = SPHERICAL_SURFACE ( 'NONE', #11095, 5.000000000000000000 ) ;
#5973 = FACE_OUTER_BOUND ( 'NONE', #10821, .T. ) ;
#5974 = CARTESIAN_POINT ( 'NONE',  ( -40.45084971874737789, 49.80000000000000426, -29.38926261462365730 ) ) ;
#5975 = CARTESIAN_POINT ( 'NONE',  ( 15.45084971874736723, 21.40000000000000213, -47.55282581475768211 ) ) ;
#5976 = CARTESIAN_POINT ( 'NONE',  ( -40.34137639590981905, 35.65937500034139873, -29.30972558990011478 ) ) ;
#5977 = CARTESIAN_POINT ( 'NONE',  ( 15.40903463028481113, 49.25937500034139305, -47.42413220539094709 ) ) ;
#5978 = CARTESIAN_POINT ( 'NONE',  ( -1.671572875253810153, 246.1715728752537871, 50.00000000000000000 ) ) ;
#5979 = FACE_OUTER_BOUND ( 'NONE', #11781, .T. ) ;
#5980 = DIRECTION ( 'NONE',  ( 1.000000000000000000, 0.000000000000000000, 0.000000000000000000 ) ) ;
#5981 =( BOUNDED_CURVE ( )  B_SPLINE_CURVE ( 3, ( #8466, #11045, #2136, #7223 ),
 .UNSPECIFIED., .F., .F. ) 
 B_SPLINE_CURVE_WITH_KNOTS ( ( 4, 4 ),
 ( 5.700094519411444516, 6.866276094947734165 ),
 .UNSPECIFIED. ) 
 CURVE ( )  GEOMETRIC_REPRESENTATION_ITEM ( )  RATIONAL_B_SPLINE_CURVE ( ( 1.000000000000000000, 0.8898432210558864242, 0.8898432210558864242, 1.000000000000000000 ) ) 
 REPRESENTATION_ITEM ( '' )  );
#5982 = DIRECTION ( 'NONE',  ( 0.000000000000000000, 1.000000000000000000, 0.000000000000000000 ) ) ;
#5983 = CARTESIAN_POINT ( 'NONE',  ( 40.45084971874737079, 42.98125000068279888, -29.38926261462366440 ) ) ;
#5984 = CARTESIAN_POINT ( 'NONE',  ( -40.45084971874737079, 42.20000000000000284, 29.38926261462367151 ) ) ;
#5985 = ORIENTED_EDGE ( 'NONE', *, *, #8173, .F. ) ;
#5987 = EDGE_CURVE ( 'NONE', #3758, #11404, #11514, .T. ) ;
#5986 = AXIS2_PLACEMENT_3D ( 'NONE', #8330, #13394, #759 ) ;
#5988 = CARTESIAN_POINT ( 'NONE',  ( 15.40903463028481113, 31.25937500034140015, -47.42413220539094709 ) ) ;
#5989 = EDGE_CURVE ( 'NONE', #13460, #891, #16425, .T. ) ;
#5990 = CARTESIAN_POINT ( 'NONE',  ( -30.90169943749473447, 48.08125000068279320, 42.53254041760200721 ) ) ;
#5991 = ORIENTED_EDGE ( 'NONE', *, *, #13801, .F. ) ;
#5992 = ORIENTED_EDGE ( 'NONE', *, *, #8035, .F. ) ;
#5993 = CARTESIAN_POINT ( 'NONE',  ( 15.45084971874736723, 41.18125000068280173, -47.55282581475768211 ) ) ;
#5994 = FACE_OUTER_BOUND ( 'NONE', #3515, .T. ) ;
#5995 = ORIENTED_EDGE ( 'NONE', *, *, #14415, .F. ) ;
#5996 = CARTESIAN_POINT ( 'NONE',  ( -50.00000000000000000, 47.78125000068279604, 0.000000000000000000 ) ) ;
#5997 = DIRECTION ( 'NONE',  ( -0.000000000000000000, -1.000000000000000000, -0.000000000000000000 ) ) ;
#5998 = CARTESIAN_POINT ( 'NONE',  ( -2.319115541017227944, 5.144547910235605315, 99.06743674540427946 ) ) ;
#5999 = DIRECTION ( 'NONE',  ( 0.000000000000000000, 0.000000000000000000, -1.000000000000000000 ) ) ;
#6000 = CARTESIAN_POINT ( 'NONE',  ( 0.000000000000000000, 267.0000000000000000, 0.000000000000000000 ) ) ;
#6001 = DIRECTION ( 'NONE',  ( 0.000000000000000000, 0.000000000000000000, -1.000000000000000000 ) ) ;
#6002 = CIRCLE ( 'NONE', #8107, 90.84711083310548929 ) ;
#6003 = CARTESIAN_POINT ( 'NONE',  ( 2.978552182361884590E-14, 47.50000000000000711, -50.00000000000000000 ) ) ;
#6004 = DIRECTION ( 'NONE',  ( -0.000000000000000000, -1.000000000000000000, -0.000000000000000000 ) ) ;
#6005 = EDGE_CURVE ( 'NONE', #9378, #4841, #110, .T. ) ;
#6006 = FACE_OUTER_BOUND ( 'NONE', #1748, .T. ) ;
#6007 = CARTESIAN_POINT ( 'NONE',  ( 50.00000000000000711, 48.68125000068279462, 16.24598481164530739 ) ) ;
#6008 = CARTESIAN_POINT ( 'NONE',  ( 7.500000000000000000, 40.00000000000000711, 39.29058411375427795 ) ) ;
#6009 = CARTESIAN_POINT ( 'NONE',  ( 9.657523855033129090E-15, 30.50000000000000000, 52.57311121191334990 ) ) ;
#6010 = CARTESIAN_POINT ( 'NONE',  ( -15.40903463028481646, 25.45937500034139589, -47.42413220539093999 ) ) ;
#6011 = CARTESIAN_POINT ( 'NONE',  ( -30.90169943749473447, 44.30000000000000426, 42.53254041760200721 ) ) ;
#6012 = LINE ( 'NONE', #1914, #12828 ) ;
#6013 = ORIENTED_EDGE ( 'NONE', *, *, #441, .F. ) ;
#6014 = CIRCLE ( 'NONE', #2802, 10.00000000000000000 ) ;
#6015 = VECTOR ( 'NONE', #12944, 1000.000000000000000 ) ;
#6016 = CARTESIAN_POINT ( 'NONE',  ( 9.877534094663406705, 8.054089844915898411, 101.0000000000000000 ) ) ;
#6017 = ORIENTED_EDGE ( 'NONE', *, *, #13167, .F. ) ;
#6018 = PRODUCT_DEFINITION_FORMATION_WITH_SPECIFIED_SOURCE ( 'ANY', '', #2806, .NOT_KNOWN. ) ;
#6019 = FACE_OUTER_BOUND ( 'NONE', #10672, .T. ) ;
#6020 = CARTESIAN_POINT ( 'NONE',  ( -30.81806926056962226, 34.15937500034139163, 42.41743335407647919 ) ) ;
#6021 = ADVANCED_FACE ( 'NONE', ( #12765 ), #1364, .F. ) ;
#6022 = DIRECTION ( 'NONE',  ( 0.8660254037844362651, 0.5000000000000041078, 0.000000000000000000 ) ) ;
#6023 = DIRECTION ( 'NONE',  ( -0.000000000000000000, -1.000000000000000000, -0.000000000000000000 ) ) ;
#6024 = LINE ( 'NONE', #14976, #4069 ) ;
#6025 = CARTESIAN_POINT ( 'NONE',  ( -16.34981105473763563, 20.27881147257167527, 102.0000000000000142 ) ) ;
#6026 = CARTESIAN_POINT ( 'NONE',  ( -40.34137639590981905, 27.72187500034139873, -29.30972558990011478 ) ) ;
#6027 = CARTESIAN_POINT ( 'NONE',  ( -49.86468353124999453, 27.75937500034139660, -16.20201782572375393 ) ) ;
#6028 = CARTESIAN_POINT ( 'NONE',  ( 17.28626291527409720, 25.00000000000000355, 18.64048258526027269 ) ) ;
#6029 = CARTESIAN_POINT ( 'NONE',  ( 49.86468353125000164, 32.92187500034139447, -6.106662507704105588E-15 ) ) ;
#6030 = AXIS2_PLACEMENT_3D ( 'NONE', #6699, #672, #13081 ) ;
#6031 = CYLINDRICAL_SURFACE ( 'NONE', #6546, 50.00000000000000000 ) ;
#6032 = CARTESIAN_POINT ( 'NONE',  ( -3.210462471511496205E-15, 45.35937500034139447, -52.43083105670540789 ) ) ;
#6033 = CARTESIAN_POINT ( 'NONE',  ( 49.86468353125000164, 40.92187500034139447, -6.106662507704105588E-15 ) ) ;
#6034 = EDGE_CURVE ( 'NONE', #7298, #11268, #14323, .T. ) ;
#6035 = CARTESIAN_POINT ( 'NONE',  ( -40.34137639590981195, 24.12187500034139731, 29.30972558990012189 ) ) ;
#6036 = ORIENTED_EDGE ( 'NONE', *, *, #7646, .T. ) ;
#6037 = CARTESIAN_POINT ( 'NONE',  ( -40.34137639590981195, 44.05937500034139731, 29.30972558990012189 ) ) ;
#6038 = CIRCLE ( 'NONE', #7873, 5.000000000000000888 ) ;
#6039 = ORIENTED_EDGE ( 'NONE', *, *, #4387, .T. ) ;
#6041 = CARTESIAN_POINT ( 'NONE',  ( -40.45084971874737079, 21.98125000068279888, 29.38926261462367151 ) ) ;
#6040 = AXIS2_PLACEMENT_3D ( 'NONE', #3761, #8905, #3 ) ;
#6042 = ORIENTED_EDGE ( 'NONE', *, *, #7339, .T. ) ;
#6043 = CARTESIAN_POINT ( 'NONE',  ( -40.45084971874737789, 33.58125000068280031, -29.38926261462365730 ) ) ;
#6044 = CARTESIAN_POINT ( 'NONE',  ( -3.210462471511496205E-15, 35.42187500034140157, -52.43083105670540789 ) ) ;
#6045 = CARTESIAN_POINT ( 'NONE',  ( -3.210462471511496205E-15, 21.35937500034139092, -52.43083105670540789 ) ) ;
#6046 = CARTESIAN_POINT ( 'NONE',  ( 7.919222016226875382, 41.44874571845315359, -49.99999999999997158 ) ) ;
#6047 = CARTESIAN_POINT ( 'NONE',  ( 40.34137639590981195, 23.12187500034139731, -29.30972558990011834 ) ) ;
#6048 = AXIS2_PLACEMENT_3D ( 'NONE', #12309, #9503, #9750 ) ;
#6049 = CARTESIAN_POINT ( 'NONE',  ( -15.45084971874737256, 31.38125000068280102, -47.55282581475767500 ) ) ;
#6050 = ADVANCED_FACE ( 'NONE', ( #3190 ), #6706, .T. ) ;
#6051 = EDGE_CURVE ( 'NONE', #11849, #5830, #13327, .T. ) ;
#6052 = CARTESIAN_POINT ( 'NONE',  ( 49.86468353125001585, 38.82187500034140015, 16.20201782572375038 ) ) ;
#6053 = CARTESIAN_POINT ( 'NONE',  ( -25.25536947722673986, 285.3889217077648368, -3.010738954466189554 ) ) ;
#6054 = ORIENTED_EDGE ( 'NONE', *, *, #7538, .F. ) ;
#6055 = CARTESIAN_POINT ( 'NONE',  ( 30.81806926056962936, 37.22187500034139873, -42.41743335407647209 ) ) ;
#6056 = CARTESIAN_POINT ( 'NONE',  ( -30.90169943749474513, 31.48125000068279533, -42.53254041760200721 ) ) ;
#6057 = ORIENTED_EDGE ( 'NONE', *, *, #7214, .F. ) ;
#6058 = VERTEX_POINT ( 'NONE', #13088 ) ;
#6059 = VECTOR ( 'NONE', #2558, 1000.000000000000227 ) ;
#6060 = ORIENTED_EDGE ( 'NONE', *, *, #10406, .F. ) ;
#6061 = CARTESIAN_POINT ( 'NONE',  ( -7.500000000000000000, 40.00000000000000711, -39.29058411375427795 ) ) ;
#6062 = CARTESIAN_POINT ( 'NONE',  ( -12.67046914267499069, 34.58135802401869086, 102.0000000000000142 ) ) ;
#6063 = CARTESIAN_POINT ( 'NONE',  ( -49.99999999999999289, 21.68125000068280528, -16.24598481164531449 ) ) ;
#6064 = CARTESIAN_POINT ( 'NONE',  ( 30.90169943749474157, 21.30000000000000426, -42.53254041760200721 ) ) ;
#6065 = CARTESIAN_POINT ( 'NONE',  ( 49.86468353125000164, 38.85937500034139447, -6.106662507704105588E-15 ) ) ;
#6066 = CARTESIAN_POINT ( 'NONE',  ( 40.34137639590981905, 42.65937500034139873, 29.30972558990010768 ) ) ;
#6067 = EDGE_CURVE ( 'NONE', #10059, #3406, #4287, .T. ) ;
#6068 = CARTESIAN_POINT ( 'NONE',  ( -40.45084971874737079, 30.20000000000000284, 29.38926261462367151 ) ) ;
#6069 = CARTESIAN_POINT ( 'NONE',  ( -30.81806926056963292, 49.62187500034139020, -42.41743335407646498 ) ) ;
#6070 = EDGE_CURVE ( 'NONE', #7551, #2664, #8185, .T. ) ;
#6071 = SURFACE_SIDE_STYLE ('',( #14856 ) ) ;
#6072 = DIRECTION ( 'NONE',  ( 0.000000000000000000, 1.000000000000000000, 0.000000000000000000 ) ) ;
#6073 = AXIS2_PLACEMENT_3D ( 'NONE', #11531, #10299, #12537 ) ;
#6074 = CARTESIAN_POINT ( 'NONE',  ( 30.90169943749473802, 41.30000000000000426, -42.53254041760200721 ) ) ;
#6075 = CARTESIAN_POINT ( 'NONE',  ( -5.179451399590974781, 14.52044592729175321, 101.0000000000000000 ) ) ;
#6076 = ORIENTED_EDGE ( 'NONE', *, *, #14840, .T. ) ;
#6077 = ADVANCED_FACE ( 'NONE', ( #13251 ), #6947, .T. ) ;
#6078 = CARTESIAN_POINT ( 'NONE',  ( 49.86468353124999453, 26.95937500034139944, -16.20201782572376459 ) ) ;
#6079 = ORIENTED_EDGE ( 'NONE', *, *, #4858, .F. ) ;
#6080 = EDGE_LOOP ( 'NONE', ( #1978, #718, #10951, #8068 ) ) ;
#6081 = VERTEX_POINT ( 'NONE', #597 ) ;
#6082 = CARTESIAN_POINT ( 'NONE',  ( 15.45084971874736723, 43.18125000068280173, -47.55282581475768211 ) ) ;
#6083 = CARTESIAN_POINT ( 'NONE',  ( -40.45084971874737079, 40.20000000000000284, 29.38926261462367151 ) ) ;
#6084 = SURFACE_SIDE_STYLE ('',( #2320 ) ) ;
#6085 = VERTEX_POINT ( 'NONE', #5692 ) ;
#6086 = CARTESIAN_POINT ( 'NONE',  ( 30.90169943749473802, 39.08125000068280031, -42.53254041760200721 ) ) ;
#6087 = DIRECTION ( 'NONE',  ( 0.9781476007338069101, -0.2079116908177532363, 0.000000000000000000 ) ) ;
#6088 = CARTESIAN_POINT ( 'NONE',  ( -5.711110298752863024, 5.918106549715473008, 98.79732775862568417 ) ) ;
#6089 = CARTESIAN_POINT ( 'NONE',  ( 0.5000000000000000000, 245.0000000000000284, 49.99999999999999289 ) ) ;
#6090 = DIRECTION ( 'NONE',  ( -0.000000000000000000, 1.000000000000000000, -0.000000000000000000 ) ) ;
#6091 = FACE_OUTER_BOUND ( 'NONE', #10889, .T. ) ;
#6092 =( BOUNDED_SURFACE ( )  B_SPLINE_SURFACE ( 3, 2, ( 
 ( #15579, #10432, #13164 ),
 ( #15488, #13247, #8258 ),
 ( #6870, #14397, #9513 ),
 ( #2943, #593, #15659 ),
 ( #4112, #3106, #5686 ),
 ( #9182, #9347, #13323 ),
 ( #13006, #11831, #5613 ),
 ( #14246, #3019, #1774 ),
 ( #11920, #6943, #14473 ),
 ( #5453, #7932, #9426 ),
 ( #11675, #10756, #520 ),
 ( #10678, #6702, #1923 ),
 ( #4360, #15730, #8181 ),
 ( #11752, #11995, #353 ),
 ( #10517, #4205, #8010 ),
 ( #13084, #1689, #10841 ),
 ( #12244, #4529, #15981 ),
 ( #2011, #16156, #6108 ) ),
 .UNSPECIFIED., .F., .F., .F. ) 
 B_SPLINE_SURFACE_WITH_KNOTS ( ( 4, 2, 2, 2, 2, 2, 2, 2, 4 ),
 ( 3, 3 ),
 ( 4.712388980384689674, 4.908738521234051966, 5.105088062083414258, 5.301437602932775661, 5.497787143782137953, 5.694136684631500245, 5.890486225480861648, 6.086835766330223940, 6.283185307179586232 ),
 ( 0.000000000000000000, 1.000000000000000000 ),
 .UNSPECIFIED. ) 
 GEOMETRIC_REPRESENTATION_ITEM ( )  RATIONAL_B_SPLINE_SURFACE ( (
 ( 1.000000000000000000, 1.000000000000000000, 1.000000000000000000),
 ( 1.000000000000000000, 1.000000000000000000, 1.000000000000000000),
 ( 1.000000000000000000, 0.9967613244521891236, 1.000000000000000000),
 ( 1.000000000000000000, 0.9841171504955514848, 1.000000000000000000),
 ( 1.000000000000000000, 0.9747108043452729076, 1.000000000000000000),
 ( 1.000000000000000000, 0.9506740354170398755, 1.000000000000000000),
 ( 1.000000000000000000, 0.9360421842396522418, 1.000000000000000000),
 ( 1.000000000000000000, 0.9031650994467438354, 1.000000000000000000),
 ( 1.000000000000000000, 0.8849191470849314678, 1.000000000000000000),
 ( 1.000000000000000000, 0.8471316604839481679, 1.000000000000000000),
 ( 1.000000000000000000, 0.8275942695274859373, 1.000000000000000000),
 ( 1.000000000000000000, 0.7902180087158534594, 1.000000000000000000),
 ( 1.000000000000000000, 0.7723968217384532542, 1.000000000000000000),
 ( 1.000000000000000000, 0.7418334179587526833, 1.000000000000000000),
 ( 1.000000000000000000, 0.7291288939600225616, 1.000000000000000000),
 ( 1.000000000000000000, 0.7117460025832956783, 1.000000000000000000),
 ( 1.000000000000000000, 0.7070717283366861894, 1.000000000000000000),
 ( 1.000000000000000000, 0.7071067811865476838, 1.000000000000000000) ) ) 
 REPRESENTATION_ITEM ( '' )  SURFACE ( )  );
#6093 = LINE ( 'NONE', #7566, #12388 ) ;
#6094 = CARTESIAN_POINT ( 'NONE',  ( -20.00000000000000355, 287.0000000000000568, -7.499999999999999112 ) ) ;
#6095 = DIRECTION ( 'NONE',  ( -0.6691306063588671194, 0.7431448254773862505, 0.000000000000000000 ) ) ;
#6096 = CARTESIAN_POINT ( 'NONE',  ( -40.45084971874737789, 45.58125000068280031, -29.38926261462365730 ) ) ;
#6097 = PLANE ( 'NONE',  #5525 ) ;
#6098 = CARTESIAN_POINT ( 'NONE',  ( -3.219174618344376363E-15, 27.50000000000000355, -52.57311121191334990 ) ) ;
#6099 = DIRECTION ( 'NONE',  ( 0.000000000000000000, 1.000000000000000000, 0.000000000000000000 ) ) ;
#6100 = CARTESIAN_POINT ( 'NONE',  ( -40.34137639590981905, 43.65937500034139163, -29.30972558990011478 ) ) ;
#6101 = VERTEX_POINT ( 'NONE', #1694 ) ;
#6102 = CARTESIAN_POINT ( 'NONE',  ( 50.00000000000000711, 44.90000000000000568, 16.24598481164530739 ) ) ;
#6103 = ORIENTED_EDGE ( 'NONE', *, *, #6195, .F. ) ;
#6104 = DIRECTION ( 'NONE',  ( 0.000000000000000000, 0.000000000000000000, -1.000000000000000000 ) ) ;
#6105 = CARTESIAN_POINT ( 'NONE',  ( 9.631387414534489405E-15, 32.35937500034139447, 52.43083105670540789 ) ) ;
#6106 = CARTESIAN_POINT ( 'NONE',  ( -2.547328955960238000E-13, 20.28125000068279959, 49.99999999999999289 ) ) ;
#6107 = LINE ( 'NONE', #14497, #10240 ) ;
#6108 = CARTESIAN_POINT ( 'NONE',  ( 20.00000000000000000, 287.0000000000000568, 7.500000000000000888 ) ) ;
#6109 = CARTESIAN_POINT ( 'NONE',  ( 40.45084971874737789, 44.58125000068280031, 29.38926261462365375 ) ) ;
#6110 = CARTESIAN_POINT ( 'NONE',  ( 40.34137639590981905, 20.72187500034139873, 29.30972558990010768 ) ) ;
#6111 = CARTESIAN_POINT ( 'NONE',  ( 40.34137639590981195, 27.05937500034139731, -29.30972558990011834 ) ) ;
#6112 = CARTESIAN_POINT ( 'NONE',  ( 50.00000000000000000, 26.78125000068279959, -6.123233995736766085E-15 ) ) ;
#6113 = CARTESIAN_POINT ( 'NONE',  ( 49.86468353125001585, 36.82187500034140015, 16.20201782572375038 ) ) ;
#6114 = DIRECTION ( 'NONE',  ( 0.8660254037844433705, 0.000000000000000000, 0.4999999999999916178 ) ) ;
#6115 = CARTESIAN_POINT ( 'NONE',  ( -15.40903463028480580, 40.25937500034139305, 47.42413220539094709 ) ) ;
#6116 = CARTESIAN_POINT ( 'NONE',  ( -49.86468353125000164, 35.92187500034140157, 0.000000000000000000 ) ) ;
#6117 = EDGE_CURVE ( 'NONE', #9016, #14633, #3210, .T. ) ;
#6118 = CARTESIAN_POINT ( 'NONE',  ( 40.45084971874737079, 43.20000000000000284, -29.38926261462366440 ) ) ;
#6119 = ORIENTED_EDGE ( 'NONE', *, *, #1740, .F. ) ;
#6120 = CARTESIAN_POINT ( 'NONE',  ( 40.34137639590981195, 41.05937500034139731, -29.30972558990011834 ) ) ;
#6121 = EDGE_LOOP ( 'NONE', ( #7382, #6800, #1353, #10798 ) ) ;
#6123 = EDGE_CURVE ( 'NONE', #1602, #15466, #9187, .T. ) ;
#6122 = CARTESIAN_POINT ( 'NONE',  ( -30.90169943749474868, 21.48125000068279533, -42.53254041760200721 ) ) ;
#6124 = ADVANCED_FACE ( 'NONE', ( #15584 ), #13010, .T. ) ;
#6125 = ORIENTED_EDGE ( 'NONE', *, *, #3967, .T. ) ;
#6126 = CARTESIAN_POINT ( 'NONE',  ( 15.45084971874736723, 41.18125000068280173, -47.55282581475768211 ) ) ;
#6127 = EDGE_CURVE ( 'NONE', #2458, #1602, #4209, .T. ) ;
#6128 = CARTESIAN_POINT ( 'NONE',  ( 49.86468353125001585, 44.82187500034138594, 16.20201782572375038 ) ) ;
#6129 = CARTESIAN_POINT ( 'NONE',  ( 9.642970592016647302, 101.1563493904846780, -1.872989114519519882 ) ) ;
#6130 = CARTESIAN_POINT ( 'NONE',  ( 9.631387414534489405E-15, 22.42187500034139802, 52.43083105670540789 ) ) ;
#6131 = CARTESIAN_POINT ( 'NONE',  ( 49.99999999999999289, 34.88125000068279746, -16.24598481164532160 ) ) ;
#6132 = CARTESIAN_POINT ( 'NONE',  ( -40.34137639590981905, 35.72187500034139163, -29.30972558990011478 ) ) ;
#6133 = CARTESIAN_POINT ( 'NONE',  ( 7.581784256837408975, 125.2766624725656897, -36.10508959731173917 ) ) ;
#6134 = CARTESIAN_POINT ( 'NONE',  ( 15.40903463028482356, 36.52187500034139589, 47.42413220539093999 ) ) ;
#6135 = CARTESIAN_POINT ( 'NONE',  ( 6.123233995736766085E-15, 51.99999999999999289, 50.00000000000000000 ) ) ;
#6136 = ORIENTED_EDGE ( 'NONE', *, *, #11659, .F. ) ;
#6137 = VERTEX_POINT ( 'NONE', #10760 ) ;
#6138 = ORIENTED_EDGE ( 'NONE', *, *, #1732, .T. ) ;
#6139 = CARTESIAN_POINT ( 'NONE',  ( 36.11321354817301454, 35.02991267065631575, 17.92868204048033931 ) ) ;
#6140 = DIRECTION ( 'NONE',  ( 0.9510565162951544194, -0.3090169943749448422, 0.000000000000000000 ) ) ;
#6141 = CARTESIAN_POINT ( 'NONE',  ( -49.99999999999999289, 21.88125000068279746, 16.24598481164533226 ) ) ;
#6142 = DIRECTION ( 'NONE',  ( 0.2079116908177531253, 0.9781476007338069101, 0.000000000000000000 ) ) ;
#6143 = CARTESIAN_POINT ( 'NONE',  ( 49.86468353125001585, 36.75937500034138594, 16.20201782572375038 ) ) ;
#6144 = CARTESIAN_POINT ( 'NONE',  ( 15.40903463028481113, 41.25937500034139305, -47.42413220539094709 ) ) ;
#6145 = DIRECTION ( 'NONE',  ( 1.000000000000000000, -0.000000000000000000, -1.734723475976807094E-17 ) ) ;
#6146 = DIRECTION ( 'NONE',  ( -0.000000000000000000, -1.000000000000000000, -0.000000000000000000 ) ) ;
#6147 = DIRECTION ( 'NONE',  ( -0.6691306063588673414, 0.7431448254773861395, 0.000000000000000000 ) ) ;
#6148 = CARTESIAN_POINT ( 'NONE',  ( -7.919222016226688865, 33.55125428154685352, -50.00000000000003553 ) ) ;
#6149 = SURFACE_STYLE_USAGE ( .BOTH. , #12538 ) ;
#6150 = ORIENTED_EDGE ( 'NONE', *, *, #5622, .T. ) ;
#6151 = CARTESIAN_POINT ( 'NONE',  ( 30.81806926056962936, 25.15937500034139518, -42.41743335407647209 ) ) ;
#6152 = EDGE_LOOP ( 'NONE', ( #14448, #7574, #8604, #2900 ) ) ;
#6153 = ORIENTED_EDGE ( 'NONE', *, *, #13021, .T. ) ;
#6154 = ORIENTED_EDGE ( 'NONE', *, *, #7135, .T. ) ;
#6155 = CARTESIAN_POINT ( 'NONE',  ( 9.657523855033129090E-15, 38.28125000068279604, 52.57311121191334990 ) ) ;
#6156 = DIRECTION ( 'NONE',  ( 0.9361168066628589024, 0.08189960831908940642, 0.3420201433256691570 ) ) ;
#6157 = ORIENTED_EDGE ( 'NONE', *, *, #5053, .T. ) ;
#6158 = DIRECTION ( 'NONE',  ( 0.000000000000000000, 0.7071067811865487940, 0.7071067811865463515 ) ) ;
#6159 = DIRECTION ( 'NONE',  ( 0.000000000000000000, 0.000000000000000000, 1.000000000000000000 ) ) ;
#6160 = FACE_OUTER_BOUND ( 'NONE', #5182, .T. ) ;
#6161 = CARTESIAN_POINT ( 'NONE',  ( 1.096031118883500133E-14, 272.0000000000000000, -89.49773270518483059 ) ) ;
#6162 = CARTESIAN_POINT ( 'NONE',  ( 40.45084971874737789, 26.58125000068279675, 29.38926261462365375 ) ) ;
#6163 = CARTESIAN_POINT ( 'NONE',  ( 0.000000000000000000, 22.50000000000000000, 101.0000000000000000 ) ) ;
#6164 = DIRECTION ( 'NONE',  ( -1.000000000000000000, 0.000000000000000000, 0.000000000000000000 ) ) ;
#6165 = EDGE_CURVE ( 'NONE', #1716, #982, #10609, .T. ) ;
#6166 = PRESENTATION_STYLE_ASSIGNMENT (( #12642 ) ) ;
#6167 = CARTESIAN_POINT ( 'NONE',  ( 0.000000000000000000, 45.07596123493892293, 0.000000000000000000 ) ) ;
#6168 = CARTESIAN_POINT ( 'NONE',  ( -40.45084971874737789, 47.58125000068280031, -29.38926261462365730 ) ) ;
#6169 = CARTESIAN_POINT ( 'NONE',  ( 7.919222016226809657, 45.22999571913594963, -50.00000000000000000 ) ) ;
#6170 = CARTESIAN_POINT ( 'NONE',  ( -40.45084971874737079, 30.20000000000000284, 29.38926261462367151 ) ) ;
#6171 = CARTESIAN_POINT ( 'NONE',  ( -30.90169943749474513, 25.69999999999999574, -42.53254041760200721 ) ) ;
#6172 = CARTESIAN_POINT ( 'NONE',  ( 41.63290517038976901, 96.34995309285439191, 5.000000000000000000 ) ) ;
#6173 = CARTESIAN_POINT ( 'NONE',  ( 40.34137639590981195, 43.05937500034139731, -29.30972558990011834 ) ) ;
#6174 = ORIENTED_EDGE ( 'NONE', *, *, #14672, .F. ) ;
#6175 = SURFACE_STYLE_USAGE ( .BOTH. , #15057 ) ;
#6176 = ORIENTED_EDGE ( 'NONE', *, *, #307, .T. ) ;
#6177 = CARTESIAN_POINT ( 'NONE',  ( -5.000000000000000000, 0.000000000000000000, 0.000000000000000000 ) ) ;
#6179 = CARTESIAN_POINT ( 'NONE',  ( -40.34137639590981905, 37.65937500034139873, -29.30972558990011478 ) ) ;
#6178 = SHAPE_REPRESENTATION ( 'BR-819', ( #4153, #14743, #11317, #16091, #10261, #10797, #3630, #12918, #1752, #2811 ), #12098 ) ;
#6180 = FACE_OUTER_BOUND ( 'NONE', #15341, .T. ) ;
#6181 = FACE_OUTER_BOUND ( 'NONE', #4462, .T. ) ;
#6182 = CARTESIAN_POINT ( 'NONE',  ( 47.34572995173812160, 25.00000000000000000, -15.64827527265554785 ) ) ;
#6183 = FACE_OUTER_BOUND ( 'NONE', #1060, .T. ) ;
#6184 = CARTESIAN_POINT ( 'NONE',  ( -30.81806926056962226, 22.22187500034139163, 42.41743335407647919 ) ) ;
#6185 = CARTESIAN_POINT ( 'NONE',  ( -49.86468353124999453, 29.75937500034139305, -16.20201782572375393 ) ) ;
#6186 = CARTESIAN_POINT ( 'NONE',  ( 1.034642314881058238E-14, 101.0808929720139417, 9.080892972013893782 ) ) ;
#6187 = CARTESIAN_POINT ( 'NONE',  ( 40.34137639590981195, 35.12187500034139731, -29.30972558990011834 ) ) ;
#6188 = FACE_OUTER_BOUND ( 'NONE', #10997, .T. ) ;
#6189 = CARTESIAN_POINT ( 'NONE',  ( -3.219174618344376363E-15, 39.49999999999999289, -52.57311121191334990 ) ) ;
#6190 = CARTESIAN_POINT ( 'NONE',  ( 9.631387414534489405E-15, 40.35937500034139447, 52.43083105670540789 ) ) ;
#6191 = CARTESIAN_POINT ( 'NONE',  ( 15.40903463028482356, 40.52187500034139589, 47.42413220539093999 ) ) ;
#6192 = CIRCLE ( 'NONE', #3531, 35.00000000000000711 ) ;
#6193 = CARTESIAN_POINT ( 'NONE',  ( -49.99999999999999289, 42.09999999999999432, 16.24598481164533226 ) ) ;
#6194 = ORIENTED_EDGE ( 'NONE', *, *, #1205, .F. ) ;
#6195 = EDGE_CURVE ( 'NONE', #13582, #3819, #11846, .T. ) ;
#6196 = CARTESIAN_POINT ( 'NONE',  ( 15.40903463028481113, 43.25937500034139305, -47.42413220539094709 ) ) ;
#6197 = EDGE_LOOP ( 'NONE', ( #3102, #6231, #1681, #7927 ) ) ;
#6198 = B_SPLINE_CURVE_WITH_KNOTS ( 'NONE', 3,
 ( #8771, #15245, #13833, #9103 ),
 .UNSPECIFIED., .F., .F.,
 ( 4, 4 ),
 ( 2.829004760702349710E-07, 0.001414802801989371557 ),
 .UNSPECIFIED. ) ;
#6199 = CARTESIAN_POINT ( 'NONE',  ( 30.90169943749475578, 26.48125000068279888, 42.53254041760200010 ) ) ;
#6200 = CARTESIAN_POINT ( 'NONE',  ( -40.45084971874737079, 34.20000000000000284, 29.38926261462367151 ) ) ;
#6201 = VECTOR ( 'NONE', #4196, 1000.000000000000000 ) ;
#6203 = ADVANCED_FACE ( 'NONE', ( #13172 ), #14330, .T. ) ;
#6202 = CARTESIAN_POINT ( 'NONE',  ( -20.00000000000000355, 307.0000000000000568, 2.500000000000001332 ) ) ;
#6204 = CARTESIAN_POINT ( 'NONE',  ( 15.40903463028481113, 45.32187500034140015, -47.42413220539094709 ) ) ;
#6205 = LINE ( 'NONE', #16334, #15534 ) ;
#6206 = CARTESIAN_POINT ( 'NONE',  ( -49.86468353124999453, 23.82187500034139305, -16.20201782572375393 ) ) ;
#6207 = CARTESIAN_POINT ( 'NONE',  ( -49.99999999999999289, 25.88125000068280102, 16.24598481164533226 ) ) ;
#6208 = EDGE_CURVE ( 'NONE', #11084, #14214, #6873, .T. ) ;
#6209 = CARTESIAN_POINT ( 'NONE',  ( -30.81806926056963292, 33.62187500034139731, -42.41743335407647209 ) ) ;
#6210 = CARTESIAN_POINT ( 'NONE',  ( -25.00000000000000711, 286.6727470533916176, -2.499999999998864908 ) ) ;
#6211 = AXIS2_PLACEMENT_3D ( 'NONE', #2237, #8484, #12304 ) ;
#6212 = CARTESIAN_POINT ( 'NONE',  ( -49.86468353124999453, 34.02187500034140299, 16.20201782572377525 ) ) ;
#6213 = CARTESIAN_POINT ( 'NONE',  ( 1.293669679204937499E-13, 41.28125000068279604, -50.00000000000000000 ) ) ;
#6214 = EDGE_LOOP ( 'NONE', ( #15009, #15360, #8495, #3451 ) ) ;
#6215 = ORIENTED_EDGE ( 'NONE', *, *, #14733, .F. ) ;
#6216 = DIRECTION ( 'NONE',  ( -0.000000000000000000, 1.000000000000000000, 0.000000000000000000 ) ) ;
#6217 = DIRECTION ( 'NONE',  ( 2.312964634635742464E-16, 0.000000000000000000, -1.000000000000000000 ) ) ;
#6218 = EDGE_CURVE ( 'NONE', #14271, #3758, #11571, .T. ) ;
#6219 = CARTESIAN_POINT ( 'NONE',  ( -7.919222016226809657, 49.33250428222964246, -49.99999999999999289 ) ) ;
#6220 = CARTESIAN_POINT ( 'NONE',  ( 9.366734789577542680E-15, 82.00000000000001421, 24.08089297201388845 ) ) ;
#6221 = CARTESIAN_POINT ( 'NONE',  ( 30.81806926056964002, 32.55937500034139731, 42.41743335407647209 ) ) ;
#6222 = DIRECTION ( 'NONE',  ( 0.000000000000000000, 0.000000000000000000, -1.000000000000000000 ) ) ;
#6223 = AXIS2_PLACEMENT_3D ( 'NONE', #8810, #10148, #4933 ) ;
#6224 = CARTESIAN_POINT ( 'NONE',  ( 15.40903463028482356, 48.52187500034140299, 47.42413220539093999 ) ) ;
#6225 = CARTESIAN_POINT ( 'NONE',  ( 5.179451399591075145, 14.52044592729181538, 102.0000000000000142 ) ) ;
#6226 = DIRECTION ( 'NONE',  ( 0.000000000000000000, 0.000000000000000000, -1.000000000000000000 ) ) ;
#6227 = ORIENTED_EDGE ( 'NONE', *, *, #14153, .T. ) ;
#6228 = EDGE_CURVE ( 'NONE', #9704, #16375, #13429, .T. ) ;
#6229 = CARTESIAN_POINT ( 'NONE',  ( -15.40903463028480580, 24.25937500034139660, 47.42413220539094709 ) ) ;
#6230 = CARTESIAN_POINT ( 'NONE',  ( -49.99999999999999289, 47.68125000068280173, -16.24598481164531449 ) ) ;
#6231 = ORIENTED_EDGE ( 'NONE', *, *, #8648, .T. ) ;
#6232 = ORIENTED_EDGE ( 'NONE', *, *, #3067, .T. ) ;
#6233 = VECTOR ( 'NONE', #3499, 1000.000000000000000 ) ;
#6234 = CARTESIAN_POINT ( 'NONE',  ( -40.45084971874737079, 35.98125000068279888, 29.38926261462367151 ) ) ;
#6235 = CARTESIAN_POINT ( 'NONE',  ( 15.45084971874737789, 34.38125000068280457, 47.55282581475767500 ) ) ;
#6236 = DIRECTION ( 'NONE',  ( 0.000000000000000000, 1.000000000000000000, 0.000000000000000000 ) ) ;
#6237 = ORIENTED_EDGE ( 'NONE', *, *, #15346, .F. ) ;
#6238 = CARTESIAN_POINT ( 'NONE',  ( -4.000000000000001776, 22.50000000000000000, 101.0000000000000000 ) ) ;
#6239 = DIRECTION ( 'NONE',  ( 1.000000000000000000, 0.000000000000000000, -2.312964634635742464E-16 ) ) ;
#6240 = CARTESIAN_POINT ( 'NONE',  ( 30.90169943749475223, 32.48125000068280599, 42.53254041760199300 ) ) ;
#6241 = DIRECTION ( 'NONE',  ( 0.000000000000000000, 0.000000000000000000, -1.000000000000000000 ) ) ;
#6242 = CARTESIAN_POINT ( 'NONE',  ( -17.35186893731094671, 20.17349094513186358, 102.0000000000000142 ) ) ;
#6243 = CARTESIAN_POINT ( 'NONE',  ( 30.27664397204019409, 40.00000000000000711, -26.14048258526078072 ) ) ;
#6244 = CARTESIAN_POINT ( 'NONE',  ( 0.000000000000000000, 22.50000000000000000, 102.0000000000000142 ) ) ;
#6245 =( NAMED_UNIT ( * ) SI_UNIT ( $, .STERADIAN. ) SOLID_ANGLE_UNIT ( ) );
#6246 = CARTESIAN_POINT ( 'NONE',  ( -9.881733417930727015, 8.048309972292139847, 101.0000000000000000 ) ) ;
#6247 = CARTESIAN_POINT ( 'NONE',  ( 40.45084971874737789, 48.58125000068280031, 29.38926261462365375 ) ) ;
#6248 = CARTESIAN_POINT ( 'NONE',  ( -2.547328955960238000E-13, 32.50000000000000000, 49.99999999999999289 ) ) ;
#6249 = VECTOR ( 'NONE', #14783, 1000.000000000000000 ) ;
#6250 = CARTESIAN_POINT ( 'NONE',  ( -49.99999999999999289, 21.90000000000000568, -16.24598481164531449 ) ) ;
#6251 = CARTESIAN_POINT ( 'NONE',  ( 49.86468353124999453, 20.95937500034138878, -16.20201782572376459 ) ) ;
#6252 = EDGE_CURVE ( 'NONE', #9264, #5867, #4037, .T. ) ;
#6253 = CARTESIAN_POINT ( 'NONE',  ( 0.000000000000000000, 52.00000000000000711, -50.00000000000000000 ) ) ;
#6254 = CARTESIAN_POINT ( 'NONE',  ( -15.40903463028481646, 43.45937500034139589, -47.42413220539093999 ) ) ;
#6255 = ORIENTED_EDGE ( 'NONE', *, *, #3159, .T. ) ;
#6256 = CARTESIAN_POINT ( 'NONE',  ( 0.000000000000000000, 193.4213562373095385, -50.00000000000000000 ) ) ;
#6257 = VERTEX_POINT ( 'NONE', #3610 ) ;
#6258 = AXIS2_PLACEMENT_3D ( 'NONE', #7201, #8596, #4974 ) ;
#6259 = CARTESIAN_POINT ( 'NONE',  ( 48.98979485566355407, 261.9999999999999432, 10.00000000000000178 ) ) ;
#6260 = B_SPLINE_CURVE_WITH_KNOTS ( 'NONE', 3,
 ( #12462, #9884, #11141, #14937 ),
 .UNSPECIFIED., .F., .F.,
 ( 4, 4 ),
 ( 0.000000000000000000, 0.01231015999390909152 ),
 .UNSPECIFIED. ) ;
#6261 = CARTESIAN_POINT ( 'NONE',  ( 40.34137639590981195, 29.05937500034139376, -29.30972558990011834 ) ) ;
#6262 = VECTOR ( 'NONE', #15444, 1000.000000000000000 ) ;
#6263 = CARTESIAN_POINT ( 'NONE',  ( 30.90169943749473802, 41.08125000068280031, -42.53254041760200721 ) ) ;
#6264 = DIRECTION ( 'NONE',  ( 0.4999999999999919509, 0.8660254037844432595, 0.000000000000000000 ) ) ;
#6265 = CARTESIAN_POINT ( 'NONE',  ( 47.55097084096160387, 25.00000000000000000, -15.01398062572901893 ) ) ;
#6266 = CARTESIAN_POINT ( 'NONE',  ( 50.00000000000000711, 30.68125000068279462, 16.24598481164530739 ) ) ;
#6267 = CARTESIAN_POINT ( 'NONE',  ( -40.34137639590981905, 25.72187500034139518, -29.30972558990011478 ) ) ;
#6268 = CARTESIAN_POINT ( 'NONE',  ( 40.34137639590981195, 23.05937500034139731, -29.30972558990011834 ) ) ;
#6269 = CARTESIAN_POINT ( 'NONE',  ( 0.000000000000000000, 22.50000000000000000, 80.00000000000000000 ) ) ;
#6270 = CARTESIAN_POINT ( 'NONE',  ( -3.210462471511496205E-15, 35.42187500034140157, -52.43083105670540789 ) ) ;
#6271 = CARTESIAN_POINT ( 'NONE',  ( -7.919222016226816763, 29.33250428222964601, -49.99999999999999289 ) ) ;
#6272 = CARTESIAN_POINT ( 'NONE',  ( 40.45084971874737789, 32.80000000000000426, 29.38926261462365375 ) ) ;
#6273 = CARTESIAN_POINT ( 'NONE',  ( 49.86468353125001585, 38.75937500034139305, 16.20201782572375038 ) ) ;
#6274 = AXIS2_PLACEMENT_3D ( 'NONE', #14262, #3203, #13024 ) ;
#6275 = CARTESIAN_POINT ( 'NONE',  ( 49.86468353125000164, 28.92187500034139802, -6.106662507704105588E-15 ) ) ;
#6276 = CIRCLE ( 'NONE', #12681, 17.50000000000000000 ) ;
#6277 = CARTESIAN_POINT ( 'NONE',  ( 30.90169943749475578, 42.69999999999999574, 42.53254041760200010 ) ) ;
#6278 = PRODUCT_DEFINITION_FORMATION_WITH_SPECIFIED_SOURCE ( 'ANY', '', #5220, .NOT_KNOWN. ) ;
#6280 = ORIENTED_EDGE ( 'NONE', *, *, #11036, .F. ) ;
#6279 =( BOUNDED_CURVE ( )  B_SPLINE_CURVE ( 2, ( #2346, #12570, #11091, #6263, #9921, #8423, #4693, #12495, #13486, #3601, #2255, #16154, #5937 ),
 .UNSPECIFIED., .F., .F. ) 
 B_SPLINE_CURVE_WITH_KNOTS ( ( 3, 2, 2, 2, 2, 2, 3 ),
 ( 0.2833333333333333814, 0.2866666666666666807, 0.2933333333333333348, 0.2999999999999999889, 0.3066666666666666430, 0.3133333333333333526, 0.3166666666666667074 ),
 .UNSPECIFIED. ) 
 CURVE ( )  GEOMETRIC_REPRESENTATION_ITEM ( )  RATIONAL_B_SPLINE_CURVE ( ( 0.9755282581475768211, 0.9755282581475770431, 1.000000000000000000, 0.9510565162951535312, 1.000000000000000000, 0.9510565162951535312, 1.000000000000000000, 0.9510565162951535312, 1.000000000000000000, 0.9510565162951535312, 1.000000000000000000, 0.9755282581475765991, 0.9755282581475768211 ) ) 
 REPRESENTATION_ITEM ( '' )  );
#6281 = CARTESIAN_POINT ( 'NONE',  ( 15.40903463028482356, 34.45937500034139589, 47.42413220539093999 ) ) ;
#6282 = EDGE_LOOP ( 'NONE', ( #13438, #11810, #14007, #4916 ) ) ;
#6283 = CARTESIAN_POINT ( 'NONE',  ( -40.34137639590981905, 45.65937500034139873, -29.30972558990011478 ) ) ;
#6284 = AXIS2_PLACEMENT_3D ( 'NONE', #7882, #14276, #7800 ) ;
#6285 = CARTESIAN_POINT ( 'NONE',  ( -40.45084971874737789, 33.80000000000000426, -29.38926261462365730 ) ) ;
#6286 = VECTOR ( 'NONE', #11486, 1000.000000000000000 ) ;
#6287 = CARTESIAN_POINT ( 'NONE',  ( -30.81806926056963292, 23.62187500034139731, -42.41743335407647209 ) ) ;
#6288 = AXIS2_PLACEMENT_3D ( 'NONE', #1921, #5852, #1086 ) ;
#6289 = CARTESIAN_POINT ( 'NONE',  ( -25.00000000000000355, 287.0000000000000568, -12.49999999999999822 ) ) ;
#6290 = CARTESIAN_POINT ( 'NONE',  ( -3.210462471511496205E-15, 45.42187500034139447, -52.43083105670540789 ) ) ;
#6291 = CARTESIAN_POINT ( 'NONE',  ( 6.725310538855729270, 29.22831317314791733, 102.0000000000000142 ) ) ;
#6292 = CARTESIAN_POINT ( 'NONE',  ( -50.00000000000000000, 46.00000000000000000, 0.000000000000000000 ) ) ;
#6293 = CARTESIAN_POINT ( 'NONE',  ( -50.00000000000000000, 29.78125000068279959, 0.000000000000000000 ) ) ;
#6294 = CARTESIAN_POINT ( 'NONE',  ( 13.19280092631089829, 34.01215678592156877, 93.07304329697090850 ) ) ;
#6295 = CARTESIAN_POINT ( 'NONE',  ( 40.34137639590981195, 37.12187500034139731, -29.30972558990011834 ) ) ;
#6296 = CARTESIAN_POINT ( 'NONE',  ( -30.00000000000000711, 282.0000000000000000, -12.49999999999999822 ) ) ;
#6297 = CIRCLE ( 'NONE', #11608, 62.25100647794772613 ) ;
#6298 = VECTOR ( 'NONE', #8066, 1000.000000000000000 ) ;
#6299 = CARTESIAN_POINT ( 'NONE',  ( -15.40903463028480580, 38.32187500034140015, 47.42413220539094709 ) ) ;
#6300 = CARTESIAN_POINT ( 'NONE',  ( 0.000000000000000000, 28.00000000000000355, 0.000000000000000000 ) ) ;
#6301 = VERTEX_POINT ( 'NONE', #9674 ) ;
#6302 = EDGE_LOOP ( 'NONE', ( #9915, #15519, #4500, #15637 ) ) ;
#6303 = FACE_OUTER_BOUND ( 'NONE', #4621, .T. ) ;
#6304 = CARTESIAN_POINT ( 'NONE',  ( 16.45433951800531247, 21.27333336794017171, 102.0000000000000142 ) ) ;
#6305 = CARTESIAN_POINT ( 'NONE',  ( 0.000000000000000000, 217.0000000000000284, 0.000000000000000000 ) ) ;
#6306 = CARTESIAN_POINT ( 'NONE',  ( 5.000000000000000000, 102.0000000000000142, 7.580410092413964129 ) ) ;
#6307 = CIRCLE ( 'NONE', #12677, 17.50000000000000000 ) ;
#6308 = CARTESIAN_POINT ( 'NONE',  ( -3.210462471511496205E-15, 31.35937500034139092, -52.43083105670540789 ) ) ;
#6309 = VECTOR ( 'NONE', #14001, 1000.000000000000000 ) ;
#6310 = SURFACE_SIDE_STYLE ('',( #15178 ) ) ;
#6311 = CIRCLE ( 'NONE', #1247, 5.000000000000000000 ) ;
#6312 = CARTESIAN_POINT ( 'NONE',  ( -15.40903463028481646, 43.52187500034139589, -47.42413220539093999 ) ) ;
#6313 = FILL_AREA_STYLE ('',( #2466 ) ) ;
#6314 = CARTESIAN_POINT ( 'NONE',  ( -40.45084971874737789, 39.80000000000000426, -29.38926261462365730 ) ) ;
#6315 = CARTESIAN_POINT ( 'NONE',  ( 8.446640517145639571E-15, 28.28125000068279959, 50.00000000000000000 ) ) ;
#6316 = CARTESIAN_POINT ( 'NONE',  ( 0.000000000000000000, 22.50000000000000000, 101.0000000000000000 ) ) ;
#6317 = ORIENTED_EDGE ( 'NONE', *, *, #12767, .F. ) ;
#6318 = EDGE_CURVE ( 'NONE', #6916, #15230, #7967, .T. ) ;
#6319 = CARTESIAN_POINT ( 'NONE',  ( -49.86468353124999453, 27.75937500034139660, -16.20201782572375393 ) ) ;
#6320 = ORIENTED_EDGE ( 'NONE', *, *, #9291, .F. ) ;
#6321 = ORIENTED_EDGE ( 'NONE', *, *, #606, .F. ) ;
#6322 = ORIENTED_EDGE ( 'NONE', *, *, #12919, .F. ) ;
#6323 = ORIENTED_EDGE ( 'NONE', *, *, #10226, .F. ) ;
#6324 = CARTESIAN_POINT ( 'NONE',  ( -20.00000000000000355, 307.0000000000000568, -7.499999999999999112 ) ) ;
#6325 = CARTESIAN_POINT ( 'NONE',  ( 0.000000000000000000, 22.50000000000000000, 102.0000000000000142 ) ) ;
#6326 = ADVANCED_FACE ( 'NONE', ( #9596 ), #14524, .F. ) ;
#6327 = ADVANCED_FACE ( 'NONE', ( #2017 ), #2352, .F. ) ;
#6328 = CARTESIAN_POINT ( 'NONE',  ( 30.90169943749475223, 28.70000000000000284, 42.53254041760199300 ) ) ;
#6329 = FACE_OUTER_BOUND ( 'NONE', #10890, .T. ) ;
#6330 = CARTESIAN_POINT ( 'NONE',  ( -15.40903463028481646, 47.45937500034139589, -47.42413220539093999 ) ) ;
#6331 = DIRECTION ( 'NONE',  ( 1.000000000000000000, 0.000000000000000000, 0.000000000000000000 ) ) ;
#6332 = FACE_OUTER_BOUND ( 'NONE', #14444, .T. ) ;
#6333 = CARTESIAN_POINT ( 'NONE',  ( -17.28626291527383785, 40.00000000000000711, 18.64048258526051427 ) ) ;
#6334 = EDGE_CURVE ( 'NONE', #10725, #2516, #3445, .T. ) ;
#6335 = AXIS2_PLACEMENT_3D ( 'NONE', #12363, #15863, #4486 ) ;
#6336 = CARTESIAN_POINT ( 'NONE',  ( 0.000000000000000000, 54.00000000000000711, 0.000000000000000000 ) ) ;
#6337 = CARTESIAN_POINT ( 'NONE',  ( -37.77664397204045343, 25.00000000000000355, 13.15010152849403369 ) ) ;
#6338 = CARTESIAN_POINT ( 'NONE',  ( 30.90169943749474157, 21.30000000000000426, -42.53254041760200721 ) ) ;
#6339 = CARTESIAN_POINT ( 'NONE',  ( 40.34137639590981905, 20.65937500034139873, 29.30972558990010768 ) ) ;
#6340 = ORIENTED_EDGE ( 'NONE', *, *, #14552, .T. ) ;
#6341 = CARTESIAN_POINT ( 'NONE',  ( 15.40903463028481113, 41.25937500034139305, -47.42413220539094709 ) ) ;
#6342 = VERTEX_POINT ( 'NONE', #8507 ) ;
#6343 = DIRECTION ( 'NONE',  ( 0.000000000000000000, 0.000000000000000000, -1.000000000000000000 ) ) ;
#6344 = EDGE_LOOP ( 'NONE', ( #5403, #4389 ) ) ;
#6345 = DIRECTION ( 'NONE',  ( -0.000000000000000000, 1.000000000000000000, -0.000000000000000000 ) ) ;
#6346 = CARTESIAN_POINT ( 'NONE',  ( 40.34137639590981905, 26.65937500034139518, 29.30972558990010768 ) ) ;
#6347 = DIRECTION ( 'NONE',  ( -1.000000000000000000, 0.000000000000000000, 0.000000000000000000 ) ) ;
#6348 = CARTESIAN_POINT ( 'NONE',  ( 0.000000000000000000, 217.0000000000000284, 0.000000000000000000 ) ) ;
#6349 = EDGE_CURVE ( 'NONE', #102, #15191, #15290, .T. ) ;
#6350 = CARTESIAN_POINT ( 'NONE',  ( 47.60088917010805432, 25.00000000000000711, -14.85495851097663333 ) ) ;
#6351 = CARTESIAN_POINT ( 'NONE',  ( -40.34137639590981195, 36.12187500034139731, 29.30972558990012189 ) ) ;
#6352 = DIRECTION ( 'NONE',  ( -6.938893903907231459E-18, 1.000000000000000000, 5.551115123125782702E-17 ) ) ;
#6353 = CARTESIAN_POINT ( 'NONE',  ( -40.34137639590981195, 26.05937500034139731, 29.30972558990012189 ) ) ;
#6354 = DIRECTION ( 'NONE',  ( 0.000000000000000000, 0.9848077530122080203, 0.1736481776669307198 ) ) ;
#6355 = ADVANCED_FACE ( 'NONE', ( #8341 ), #10845, .F. ) ;
#6356 = CARTESIAN_POINT ( 'NONE',  ( -40.34137639590981905, 35.72187500034139163, -29.30972558990011478 ) ) ;
#6357 = DIRECTION ( 'NONE',  ( 0.000000000000000000, 0.000000000000000000, -1.000000000000000000 ) ) ;
#6358 = CIRCLE ( 'NONE', #15633, 40.00000000000000000 ) ;
#6359 = CARTESIAN_POINT ( 'NONE',  ( -40.45084971874737789, 31.80000000000000071, -29.38926261462365730 ) ) ;
#6360 = CARTESIAN_POINT ( 'NONE',  ( 30.81806926056964002, 36.55937500034139731, 42.41743335407647209 ) ) ;
#6361 = CARTESIAN_POINT ( 'NONE',  ( -15.40903463028480580, 28.32187500034139660, 47.42413220539094709 ) ) ;
#6362 = CARTESIAN_POINT ( 'NONE',  ( -15.45084971874736368, 46.40000000000000568, 47.55282581475768211 ) ) ;
#6363 = EDGE_LOOP ( 'NONE', ( #2293, #3491 ) ) ;
#6364 = EDGE_LOOP ( 'NONE', ( #12394, #2899, #3415, #1134 ) ) ;
#6365 = CARTESIAN_POINT ( 'NONE',  ( -49.86468353124999453, 35.75937500034139305, -16.20201782572375393 ) ) ;
#6366 = VERTEX_POINT ( 'NONE', #12167 ) ;
#6367 = CARTESIAN_POINT ( 'NONE',  ( 25.03223043949687820, 286.3455096218830249, -2.564460878999441196 ) ) ;
#6368 = CARTESIAN_POINT ( 'NONE',  ( -40.34137639590981905, 47.65937500034139873, -29.30972558990011478 ) ) ;
#6369 = DIRECTION ( 'NONE',  ( 0.000000000000000000, 1.000000000000000000, 0.000000000000000000 ) ) ;
#6370 = CARTESIAN_POINT ( 'NONE',  ( -30.81806926056963292, 21.62187500034139376, -42.41743335407647209 ) ) ;
#6371 = CARTESIAN_POINT ( 'NONE',  ( -3.918041248536338728, 6.471932344328960696, 102.0000000000000142 ) ) ;
#6372 = CARTESIAN_POINT ( 'NONE',  ( -40.34137639590981195, 40.12187500034139731, 29.30972558990012189 ) ) ;
#6373 = CARTESIAN_POINT ( 'NONE',  ( 17.45639740057861644, 21.16801284050037424, 102.0000000000000142 ) ) ;
#6374 = EDGE_CURVE ( 'NONE', #10461, #10320, #2309, .T. ) ;
#6375 = CARTESIAN_POINT ( 'NONE',  ( 30.81806926056964002, 20.62187500034139020, 42.41743335407647209 ) ) ;
#6376 = ADVANCED_FACE ( 'NONE', ( #7187 ), #10249, .T. ) ;
#6377 = CARTESIAN_POINT ( 'NONE',  ( 15.45084971874736723, 27.18125000068279817, -47.55282581475768211 ) ) ;
#6378 = CARTESIAN_POINT ( 'NONE',  ( 2.291013771646459141, 39.88729579110228229, 92.94536576005377526 ) ) ;
#6379 =( BOUNDED_CURVE ( )  B_SPLINE_CURVE ( 2, ( #6918, #14209, #7986, #4414, #408, #12981, #8156, #6845, #12893, #5352, #4083, #1823, #5662 ),
 .UNSPECIFIED., .F., .F. ) 
 B_SPLINE_CURVE_WITH_KNOTS ( ( 3, 2, 2, 2, 2, 2, 3 ),
 ( 0.2166666666666666741, 0.2200000000000000011, 0.2266666666666666552, 0.2333333333333333370, 0.2399999999999999911, 0.2466666666666666730, 0.2500000000000000000 ),
 .UNSPECIFIED. ) 
 CURVE ( )  GEOMETRIC_REPRESENTATION_ITEM ( )  RATIONAL_B_SPLINE_CURVE ( ( 0.9755282581475768211, 0.9755282581475768211, 1.000000000000000000, 0.9510565162951535312, 1.000000000000000000, 0.9510565162951535312, 1.000000000000000000, 0.9510565162951535312, 1.000000000000000000, 0.9510565162951535312, 1.000000000000000000, 0.9755282581475768211, 0.9755282581475765991 ) ) 
 REPRESENTATION_ITEM ( '' )  );
#6380 = AXIS2_PLACEMENT_3D ( 'NONE', #14518, #552, #15690 ) ;
#6381 = CARTESIAN_POINT ( 'NONE',  ( -49.86468353124999453, 34.02187500034140299, 16.20201782572377525 ) ) ;
#6382 = CARTESIAN_POINT ( 'NONE',  ( 1.293669679204937499E-13, 39.28125000068280315, -50.00000000000000000 ) ) ;
#6383 = DIRECTION ( 'NONE',  ( 0.000000000000000000, 1.000000000000000000, 0.000000000000000000 ) ) ;
#6384 = VERTEX_POINT ( 'NONE', #180 ) ;
#6385 = VERTEX_POINT ( 'NONE', #3850 ) ;
#6386 = CARTESIAN_POINT ( 'NONE',  ( -25.00000000000000355, 287.0000000000000568, 12.50000000000000000 ) ) ;
#6387 = CARTESIAN_POINT ( 'NONE',  ( -25.00000000000000355, 312.0000000000000568, 2.500000000000001332 ) ) ;
#6388 = DIRECTION ( 'NONE',  ( 0.000000000000000000, 1.000000000000000000, 0.000000000000000000 ) ) ;
#6389 = CARTESIAN_POINT ( 'NONE',  ( -40.34137639590981195, 34.05937500034139731, 29.30972558990012189 ) ) ;
#6390 = SURFACE_STYLE_USAGE ( .BOTH. , #6310 ) ;
#6391 = CARTESIAN_POINT ( 'NONE',  ( 40.34137639590981905, 46.72187500034139873, 29.30972558990010768 ) ) ;
#6392 = SURFACE_SIDE_STYLE ('',( #3892 ) ) ;
#6393 = CARTESIAN_POINT ( 'NONE',  ( 3.918041248536554555, 6.471932344329013098, 102.0000000000000142 ) ) ;
#6394 = CARTESIAN_POINT ( 'NONE',  ( 19.48557158514982035, 33.75000000000009237, 101.0000000000000000 ) ) ;
#6395 = CARTESIAN_POINT ( 'NONE',  ( -8.477241335952138357, 18.18301270189218855, 102.0000000000000142 ) ) ;
#6396 = ORIENTED_EDGE ( 'NONE', *, *, #213, .T. ) ;
#6397 = CARTESIAN_POINT ( 'NONE',  ( -40.34137639590981195, 22.05937500034139731, 29.30972558990012189 ) ) ;
#6398 = ORIENTED_EDGE ( 'NONE', *, *, #14511, .F. ) ;
#6399 = CARTESIAN_POINT ( 'NONE',  ( -40.45084971874737079, 45.98125000068279888, 29.38926261462367151 ) ) ;
#6400 = VERTEX_POINT ( 'NONE', #5040 ) ;
#6401 = ORIENTED_EDGE ( 'NONE', *, *, #3975, .T. ) ;
#6402 = CARTESIAN_POINT ( 'NONE',  ( -2.445080149700054274E-14, 46.50000000000000711, 50.00000000000000000 ) ) ;
#6403 = CARTESIAN_POINT ( 'NONE',  ( 4.126043002969939977, 5.493361027597405410, 101.0000000000000000 ) ) ;
#6404 = CARTESIAN_POINT ( 'NONE',  ( -7.919222016226816763, 27.55125428154684641, -49.99999999999999289 ) ) ;
#6405 = DIRECTION ( 'NONE',  ( 0.000000000000000000, 0.000000000000000000, -1.000000000000000000 ) ) ;
#6406 = CARTESIAN_POINT ( 'NONE',  ( -0.4999999999999998890, 38.99242250247064590, 102.0000000000000142 ) ) ;
#6407 = DIRECTION ( 'NONE',  ( 0.000000000000000000, 1.000000000000000000, 0.000000000000000000 ) ) ;
#6408 = FACE_OUTER_BOUND ( 'NONE', #6814, .T. ) ;
#6409 = DIRECTION ( 'NONE',  ( 0.000000000000000000, 0.000000000000000000, 1.000000000000000000 ) ) ;
#6410 =( NAMED_UNIT ( * ) PLANE_ANGLE_UNIT ( ) SI_UNIT ( $, .RADIAN. ) );
#6411 = CARTESIAN_POINT ( 'NONE',  ( -49.99999999999999289, 49.89999999999999147, -16.24598481164531449 ) ) ;
#6412 = CARTESIAN_POINT ( 'NONE',  ( -15.45084971874737256, 43.38125000068279746, -47.55282581475767500 ) ) ;
#6413 = DIRECTION ( 'NONE',  ( 0.000000000000000000, 0.000000000000000000, -1.000000000000000000 ) ) ;
#6414 = CARTESIAN_POINT ( 'NONE',  ( -40.45084971874737789, 21.80000000000000071, -29.38926261462365730 ) ) ;
#6415 = CARTESIAN_POINT ( 'NONE',  ( 0.000000000000000000, 242.0000000000000284, 0.000000000000000000 ) ) ;
#6416 = ADVANCED_FACE ( 'NONE', ( #10335 ), #1094, .F. ) ;
#6417 = ORIENTED_EDGE ( 'NONE', *, *, #8241, .T. ) ;
#6418 = EDGE_CURVE ( 'NONE', #3981, #14778, #5641, .T. ) ;
#6419 = CARTESIAN_POINT ( 'NONE',  ( 30.81806926056962936, 45.15937500034139873, -42.41743335407647209 ) ) ;
#6420 = ORIENTED_EDGE ( 'NONE', *, *, #8343, .F. ) ;
#6421 = DIRECTION ( 'NONE',  ( 0.000000000000000000, 0.000000000000000000, -1.000000000000000000 ) ) ;
#6422 = EDGE_CURVE ( 'NONE', #15026, #6818, #12821, .T. ) ;
#6423 = CYLINDRICAL_SURFACE ( 'NONE', #10015, 50.00000000000000000 ) ;
#6424 = CARTESIAN_POINT ( 'NONE',  ( -49.86468353125000164, 25.85937500034139802, 0.000000000000000000 ) ) ;
#6425 = ORIENTED_EDGE ( 'NONE', *, *, #6051, .F. ) ;
#6426 = CARTESIAN_POINT ( 'NONE',  ( 50.00000000000000711, 32.89999999999999858, 16.24598481164530739 ) ) ;
#6427 = CARTESIAN_POINT ( 'NONE',  ( 0.000000000000000000, 20.00000000000000355, 0.000000000000000000 ) ) ;
#6428 = CARTESIAN_POINT ( 'NONE',  ( 47.44954343046539691, 25.00000000000000000, -15.33151233206056041 ) ) ;
#6429 = CARTESIAN_POINT ( 'NONE',  ( -49.86468353124999453, 35.82187500034139305, -16.20201782572375393 ) ) ;
#6430 = ADVANCED_FACE ( 'NONE', ( #9085, #2678 ), #14141, .T. ) ;
#6431 = CARTESIAN_POINT ( 'NONE',  ( 40.45084971874737079, 30.98125000068279888, -29.38926261462366440 ) ) ;
#6432 = CARTESIAN_POINT ( 'NONE',  ( 49.86468353124999453, 20.95937500034139234, -16.20201782572376104 ) ) ;
#6433 = FACE_OUTER_BOUND ( 'NONE', #16228, .T. ) ;
#6434 = CARTESIAN_POINT ( 'NONE',  ( -15.40903463028480580, 26.32187500034140015, 47.42413220539094709 ) ) ;
#6435 = CARTESIAN_POINT ( 'NONE',  ( -7.394441145214675437, 28.48516834767043093, 102.0000000000000142 ) ) ;
#6436 = CARTESIAN_POINT ( 'NONE',  ( -40.45084971874737079, 32.20000000000000284, 29.38926261462367151 ) ) ;
#6437 = CARTESIAN_POINT ( 'NONE',  ( -15.40903463028480580, 36.25937500034140015, 47.42413220539094709 ) ) ;
#6438 = CARTESIAN_POINT ( 'NONE',  ( 49.86468353125001585, 30.82187500034139660, 16.20201782572375038 ) ) ;
#6439 = CARTESIAN_POINT ( 'NONE',  ( -30.90169943749473802, 46.30000000000000426, 42.53254041760200721 ) ) ;
#6440 = ORIENTED_EDGE ( 'NONE', *, *, #10727, .T. ) ;
#6441 = ORIENTED_EDGE ( 'NONE', *, *, #12831, .T. ) ;
#6442 = EDGE_CURVE ( 'NONE', #4234, #14778, #8753, .T. ) ;
#6443 = UNCERTAINTY_MEASURE_WITH_UNIT (LENGTH_MEASURE( 1.000000000000000082E-05 ), #5094, 'distance_accuracy_value', 'NONE');
#6444 = CARTESIAN_POINT ( 'NONE',  ( 9.631387414534489405E-15, 36.35937500034140157, 52.43083105670540789 ) ) ;
#6445 = ORIENTED_EDGE ( 'NONE', *, *, #14339, .F. ) ;
#6446 = ORIENTED_EDGE ( 'NONE', *, *, #13630, .T. ) ;
#6447 = CARTESIAN_POINT ( 'NONE',  ( 25.00000000000000711, 287.0000000000000000, -7.500000000000000888 ) ) ;
#6448 = CARTESIAN_POINT ( 'NONE',  ( -49.86468353125000164, 49.85937500034139447, 0.000000000000000000 ) ) ;
#6449 = LINE ( 'NONE', #13829, #7293 ) ;
#6450 = CARTESIAN_POINT ( 'NONE',  ( 49.86468353124999453, 27.02187500034139589, -16.20201782572376459 ) ) ;
#6451 = EDGE_CURVE ( 'NONE', #15954, #3182, #1342, .T. ) ;
#6452 = CARTESIAN_POINT ( 'NONE',  ( 2.500000000000000000, 247.0000000000000284, 40.00000000000000000 ) ) ;
#6453 = CARTESIAN_POINT ( 'NONE',  ( -30.81806926056962226, 44.22187500034139163, 42.41743335407647919 ) ) ;
#6454 = CARTESIAN_POINT ( 'NONE',  ( -40.34137639590981905, 39.65937500034139873, -29.30972558990011478 ) ) ;
#6455 = CARTESIAN_POINT ( 'NONE',  ( -16.79799753235266735, 27.43226914341395783, 101.0000000000000000 ) ) ;
#6456 = CARTESIAN_POINT ( 'NONE',  ( 49.99999999999999289, 45.10000000000000853, -16.24598481164532160 ) ) ;
#6457 = AXIS2_PLACEMENT_3D ( 'NONE', #3732, #3487, #1222 ) ;
#6458 = CARTESIAN_POINT ( 'NONE',  ( -40.45084971874737079, 29.98125000068279888, 29.38926261462367151 ) ) ;
#6459 = CARTESIAN_POINT ( 'NONE',  ( -3.210462471511496205E-15, 49.42187500034138736, -52.43083105670540789 ) ) ;
#6460 = CARTESIAN_POINT ( 'NONE',  ( 9.631387414534489405E-15, 34.42187500034138736, 52.43083105670540789 ) ) ;
#6461 = CARTESIAN_POINT ( 'NONE',  ( 0.1743114854953164983, 100.0076106038165165, 5.000000000000000000 ) ) ;
#6462 = ORIENTED_EDGE ( 'NONE', *, *, #13945, .F. ) ;
#6463 = VECTOR ( 'NONE', #8450, 1000.000000000000114 ) ;
#6464 = ORIENTED_EDGE ( 'NONE', *, *, #112, .T. ) ;
#6465 = CARTESIAN_POINT ( 'NONE',  ( -12.66515988160626982, 34.57657754388018390, 101.0000000000000000 ) ) ;
#6466 = CARTESIAN_POINT ( 'NONE',  ( -14.90544456622763470, 13.31698729810771376, 101.0000000000000000 ) ) ;
#6467 = FACE_OUTER_BOUND ( 'NONE', #10361, .T. ) ;
#6468 = CARTESIAN_POINT ( 'NONE',  ( -30.81806926056962226, 48.22187500034139163, 42.41743335407647209 ) ) ;
#6469 = CARTESIAN_POINT ( 'NONE',  ( 40.34137639590981195, 33.05937500034139731, -29.30972558990011834 ) ) ;
#6470 = LINE ( 'NONE', #5240, #7943 ) ;
#6471 =( BOUNDED_CURVE ( )  B_SPLINE_CURVE ( 2, ( #4746, #635, #5895, #11136, #14932, #13531, #12033, #884, #16023, #4826, #15867, #2133, #7222 ),
 .UNSPECIFIED., .F., .T. ) 
 B_SPLINE_CURVE_WITH_KNOTS ( ( 3, 2, 2, 2, 2, 2, 3 ),
 ( 0.8166666666666666519, 0.8199999999999999512, 0.8266666666666666607, 0.8333333333333333703, 0.8399999999999999689, 0.8466666666666666785, 0.8500000000000000888 ),
 .UNSPECIFIED. ) 
 CURVE ( )  GEOMETRIC_REPRESENTATION_ITEM ( )  RATIONAL_B_SPLINE_CURVE ( ( 0.9755282581475768211, 0.9755282581475768211, 1.000000000000000000, 0.9510565162951535312, 1.000000000000000000, 0.9510565162951535312, 1.000000000000000000, 0.9510565162951535312, 1.000000000000000000, 0.9510565162951535312, 1.000000000000000000, 0.9755282581475763770, 0.9755282581475768211 ) ) 
 REPRESENTATION_ITEM ( '' )  );
#6472 = CARTESIAN_POINT ( 'NONE',  ( -30.81806926056962226, 46.22187500034139163, 42.41743335407647209 ) ) ;
#6473 = DIRECTION ( 'NONE',  ( 0.000000000000000000, 0.000000000000000000, 1.000000000000000000 ) ) ;
#6474 = AXIS2_PLACEMENT_3D ( 'NONE', #14877, #7250, #660 ) ;
#6475 = DIRECTION ( 'NONE',  ( -0.000000000000000000, -1.000000000000000000, -0.000000000000000000 ) ) ;
#6476 = ORIENTED_EDGE ( 'NONE', *, *, #12382, .T. ) ;
#6477 = CARTESIAN_POINT ( 'NONE',  ( -30.81806926056963292, 47.62187500034139731, -42.41743335407647209 ) ) ;
#6478 = ORIENTED_EDGE ( 'NONE', *, *, #213, .F. ) ;
#6479 = DIRECTION ( 'NONE',  ( 1.000000000000000000, 0.000000000000000000, 0.000000000000000000 ) ) ;
#6480 = ORIENTED_EDGE ( 'NONE', *, *, #1427, .F. ) ;
#6481 = EDGE_LOOP ( 'NONE', ( #7683, #1200, #10557, #1790 ) ) ;
#6482 = ADVANCED_FACE ( 'NONE', ( #15143 ), #11420, .F. ) ;
#6483 = PLANE ( 'NONE',  #8961 ) ;
#6484 = PLANE ( 'NONE',  #8609 ) ;
#6485 = VECTOR ( 'NONE', #14603, 1000.000000000000000 ) ;
#6486 = FACE_OUTER_BOUND ( 'NONE', #2839, .T. ) ;
#6487 = DIRECTION ( 'NONE',  ( -0.000000000000000000, 0.000000000000000000, 1.000000000000000000 ) ) ;
#6488 = CARTESIAN_POINT ( 'NONE',  ( 15.40903463028482356, 48.45937500034140299, 47.42413220539093999 ) ) ;
#6489 = CARTESIAN_POINT ( 'NONE',  ( -2.500000000000000000, 242.0000000000000284, -47.99999999999999289 ) ) ;
#6490 = CARTESIAN_POINT ( 'NONE',  ( 30.90169943749473802, 27.08125000068280031, -42.53254041760200721 ) ) ;
#6491 = CYLINDRICAL_SURFACE ( 'NONE', #12180, 40.00000000000000000 ) ;
#6492 =( NAMED_UNIT ( * ) PLANE_ANGLE_UNIT ( ) SI_UNIT ( $, .RADIAN. ) );
#6493 = CARTESIAN_POINT ( 'NONE',  ( 10.09851121871635904, 9.451242543235769844, 102.0000000000000142 ) ) ;
#6494 = CARTESIAN_POINT ( 'NONE',  ( 40.45084971874737789, 38.58125000068280031, 29.38926261462365375 ) ) ;
#6495 = DIRECTION ( 'NONE',  ( -0.9135454576426060846, 0.4067366430757887730, 0.000000000000000000 ) ) ;
#6496 = CARTESIAN_POINT ( 'NONE',  ( -15.45084971874736368, 22.39999999999999858, 47.55282581475768211 ) ) ;
#6497 = EDGE_CURVE ( 'NONE', #1275, #305, #6820, .T. ) ;
#6498 = PLANE ( 'NONE',  #10161 ) ;
#6499 = VERTEX_POINT ( 'NONE', #1174 ) ;
#6500 = AXIS2_PLACEMENT_3D ( 'NONE', #1279, #6369, #10186 ) ;
#6501 = CARTESIAN_POINT ( 'NONE',  ( 9.631387414534489405E-15, 40.35937500034139447, 52.43083105670540789 ) ) ;
#6502 = ORIENTED_EDGE ( 'NONE', *, *, #12401, .T. ) ;
#6503 = DIRECTION ( 'NONE',  ( -6.938893903907231459E-18, 1.000000000000000000, 5.551115123125782702E-17 ) ) ;
#6504 = DIRECTION ( 'NONE',  ( -6.938893903907231459E-18, 1.000000000000000000, 5.551115123125782702E-17 ) ) ;
#6505 = CARTESIAN_POINT ( 'NONE',  ( -49.86468353125000164, 31.85937500034139447, 0.000000000000000000 ) ) ;
#6506 = ORIENTED_EDGE ( 'NONE', *, *, #5809, .T. ) ;
#6507 = FACE_OUTER_BOUND ( 'NONE', #15832, .T. ) ;
#6509 = EDGE_CURVE ( 'NONE', #646, #9440, #4717, .T. ) ;
#6508 = LINE ( 'NONE', #10412, #15809 ) ;
#6510 = CARTESIAN_POINT ( 'NONE',  ( 46.96694430692144095, 25.00000000000000000, -16.75173377947149689 ) ) ;
#6511 = CARTESIAN_POINT ( 'NONE',  ( -15.40903463028481646, 33.52187500034140299, -47.42413220539093999 ) ) ;
#6512 = AXIS2_PLACEMENT_3D ( 'NONE', #4004, #6503, #2745 ) ;
#6513 = CARTESIAN_POINT ( 'NONE',  ( 0.000000000000000000, 20.00000000000000355, 50.00000000000000000 ) ) ;
#6514 = CARTESIAN_POINT ( 'NONE',  ( 49.86468353125001585, 20.75937500034140015, 16.20201782572375038 ) ) ;
#6515 = CARTESIAN_POINT ( 'NONE',  ( 0.000000000000000000, 193.4213562373095385, 0.000000000000000000 ) ) ;
#6516 = CARTESIAN_POINT ( 'NONE',  ( -15.40903463028480580, 30.32187500034140015, 47.42413220539094709 ) ) ;
#6517 = DIRECTION ( 'NONE',  ( 0.000000000000000000, 1.000000000000000000, 0.000000000000000000 ) ) ;
#6518 = CARTESIAN_POINT ( 'NONE',  ( 40.45084971874737789, 28.80000000000000426, 29.38926261462365375 ) ) ;
#6519 = CARTESIAN_POINT ( 'NONE',  ( 40.34137639590981195, 35.05937500034139731, -29.30972558990011834 ) ) ;
#6520 = CARTESIAN_POINT ( 'NONE',  ( -30.81806926056963292, 33.62187500034139731, -42.41743335407647209 ) ) ;
#6521 = B_SPLINE_CURVE_WITH_KNOTS ( 'NONE', 3,
 ( #60, #5165, #1394, #15275 ),
 .UNSPECIFIED., .F., .F.,
 ( 4, 4 ),
 ( 0.01002676606614814371, 0.01717959331248046853 ),
 .UNSPECIFIED. ) ;
#6522 = ORIENTED_EDGE ( 'NONE', *, *, #15590, .F. ) ;
#6523 = AXIS2_PLACEMENT_3D ( 'NONE', #3035, #2959, #8106 ) ;
#6524 = EDGE_CURVE ( 'NONE', #3201, #6897, #5115, .T. ) ;
#6525 = CARTESIAN_POINT ( 'NONE',  ( -15.40903463028480580, 34.25937500034139305, 47.42413220539094709 ) ) ;
#6526 = EDGE_LOOP ( 'NONE', ( #1145, #10974, #1476, #5160 ) ) ;
#6527 = ORIENTED_EDGE ( 'NONE', *, *, #3477, .F. ) ;
#6528 = CARTESIAN_POINT ( 'NONE',  ( 25.25536947722733672, 285.3889217077634726, -3.010738954466163353 ) ) ;
#6529 = CARTESIAN_POINT ( 'NONE',  ( -30.81806926056962226, 48.15937500034139873, 42.41743335407647919 ) ) ;
#6530 = CARTESIAN_POINT ( 'NONE',  ( -2.547328955960238000E-13, 34.50000000000000000, 49.99999999999999289 ) ) ;
#6531 = CARTESIAN_POINT ( 'NONE',  ( 49.86468353125001585, 24.82187500034139305, 16.20201782572375038 ) ) ;
#6532 = CARTESIAN_POINT ( 'NONE',  ( -3.078562342020560116, 5.611635739450979266, 101.3333374614808662 ) ) ;
#6533 = CARTESIAN_POINT ( 'NONE',  ( 9.631387414534489405E-15, 36.42187500034139447, 52.43083105670540789 ) ) ;
#6534 = CARTESIAN_POINT ( 'NONE',  ( 40.34137639590981195, 45.05937500034139731, -29.30972558990011834 ) ) ;
#6535 = CARTESIAN_POINT ( 'NONE',  ( -3.111920190527341144E-15, 35.50000000000000000, -50.00000000000000000 ) ) ;
#6536 = VECTOR ( 'NONE', #7166, 1000.000000000000000 ) ;
#6537 = CARTESIAN_POINT ( 'NONE',  ( 15.45084971874736723, 47.40000000000000568, -47.55282581475768211 ) ) ;
#6538 = EDGE_CURVE ( 'NONE', #7158, #11087, #13, .T. ) ;
#6539 = PRODUCT_DEFINITION_SHAPE ( 'NONE', 'NONE',  #16472 ) ;
#6540 = CARTESIAN_POINT ( 'NONE',  ( -30.90169943749474868, 29.48125000068279888, -42.53254041760200721 ) ) ;
#6541 = APPLICATION_CONTEXT ( 'automotive_design' ) ;
#6542 = CARTESIAN_POINT ( 'NONE',  ( 1.152251941144751379, 40.00000000000000711, 92.94692077166136812 ) ) ;
#6543 = STYLED_ITEM ( 'NONE', ( #4403 ), #8007 ) ;
#6544 = CARTESIAN_POINT ( 'NONE',  ( -15.40903463028480580, 28.32187500034139660, 47.42413220539094709 ) ) ;
#6545 = CARTESIAN_POINT ( 'NONE',  ( -7.580410092413979228, 102.0000000000000142, -5.000000000000000000 ) ) ;
#6546 = AXIS2_PLACEMENT_3D ( 'NONE', #1017, #8676, #11102 ) ;
#6547 = VERTEX_POINT ( 'NONE', #7674 ) ;
#6548 = AXIS2_PLACEMENT_3D ( 'NONE', #9799, #11132, #9957 ) ;
#6549 = VECTOR ( 'NONE', #15980, 1000.000000000000000 ) ;
#6551 = CARTESIAN_POINT ( 'NONE',  ( 30.90169943749475578, 36.48125000068279888, 42.53254041760200010 ) ) ;
#6550 = AXIS2_PLACEMENT_3D ( 'NONE', #12160, #16152, #15978 ) ;
#6552 = VECTOR ( 'NONE', #5017, 1000.000000000000000 ) ;
#6553 = ORIENTED_EDGE ( 'NONE', *, *, #14934, .T. ) ;
#6554 = CARTESIAN_POINT ( 'NONE',  ( 30.90169943749473802, 49.08125000068280031, -42.53254041760200721 ) ) ;
#6555 = CARTESIAN_POINT ( 'NONE',  ( -5.000000000000000000, 92.00000000000001421, 0.000000000000000000 ) ) ;
#6556 = CARTESIAN_POINT ( 'NONE',  ( 4.716203841691264387, 99.57974595388792238, -8.487905985326161584 ) ) ;
#6557 = CARTESIAN_POINT ( 'NONE',  ( -15.40903463028481646, 45.52187500034139589, -47.42413220539093999 ) ) ;
#6558 = CARTESIAN_POINT ( 'NONE',  ( 30.81806926056962936, 31.15937500034139518, -42.41743335407647209 ) ) ;
#6559 = ADVANCED_FACE ( 'NONE', ( #6433 ), #12745, .F. ) ;
#6560 = DIRECTION ( 'NONE',  ( -0.000000000000000000, -1.000000000000000000, -0.000000000000000000 ) ) ;
#6561 = DIRECTION ( 'NONE',  ( 1.224646799147353207E-16, -1.000000000000000000, 0.000000000000000000 ) ) ;
#6562 = EDGE_CURVE ( 'NONE', #4835, #10619, #12907, .T. ) ;
#6563 = CARTESIAN_POINT ( 'NONE',  ( 49.86468353124999453, 49.02187500034140299, -16.20201782572376104 ) ) ;
#6564 = DIRECTION ( 'NONE',  ( 0.000000000000000000, 0.000000000000000000, 1.000000000000000000 ) ) ;
#6565 = DIRECTION ( 'NONE',  ( -0.9993309688977879413, 0.03657341386592747462, 0.000000000000000000 ) ) ;
#6566 = VECTOR ( 'NONE', #8975, 1000.000000000000000 ) ;
#6567 = CARTESIAN_POINT ( 'NONE',  ( 40.34137639590981905, 48.72187500034139873, 29.30972558990010768 ) ) ;
#6568 = CARTESIAN_POINT ( 'NONE',  ( 0.000000000000000000, 22.50000000000000000, 101.0000000000000000 ) ) ;
#6569 = ORIENTED_EDGE ( 'NONE', *, *, #9105, .F. ) ;
#6570 = CARTESIAN_POINT ( 'NONE',  ( -49.86468353124999453, 46.02187500034140299, 16.20201782572377525 ) ) ;
#6571 = VERTEX_POINT ( 'NONE', #4094 ) ;
#6572 = CARTESIAN_POINT ( 'NONE',  ( -47.28673853953969797, 260.3313524089090265, -10.00000000000000178 ) ) ;
#6573 = EDGE_LOOP ( 'NONE', ( #118, #13201 ) ) ;
#6574 = ORIENTED_EDGE ( 'NONE', *, *, #1781, .T. ) ;
#6575 = VECTOR ( 'NONE', #2138, 1000.000000000000000 ) ;
#6576 = DIRECTION ( 'NONE',  ( -0.000000000000000000, -1.000000000000000000, -0.000000000000000000 ) ) ;
#6577 = CARTESIAN_POINT ( 'NONE',  ( 7.919222016226758143, 38.33250428222964246, 50.00000000000000711 ) ) ;
#6579 =( BOUNDED_CURVE ( )  B_SPLINE_CURVE ( 2, ( #7146, #3308, #8375, #12282, #6068, #10806, #14854, #8615, #13450, #9554, #8537, #12123, #7309 ),
 .UNSPECIFIED., .F., .T. ) 
 B_SPLINE_CURVE_WITH_KNOTS ( ( 3, 2, 2, 2, 2, 2, 3 ),
 ( 0.6500000000000000222, 0.6533333333333333215, 0.6600000000000000311, 0.6666666666666666297, 0.6733333333333333393, 0.6800000000000000488, 0.6833333333333333481 ),
 .UNSPECIFIED. ) 
 CURVE ( )  GEOMETRIC_REPRESENTATION_ITEM ( )  RATIONAL_B_SPLINE_CURVE ( ( 0.9755282581475768211, 0.9755282581475771542, 1.000000000000000000, 0.9510565162951535312, 1.000000000000000000, 0.9510565162951535312, 1.000000000000000000, 0.9510565162951535312, 1.000000000000000000, 0.9510565162951535312, 1.000000000000000000, 0.9755282581475768211, 0.9755282581475768211 ) ) 
 REPRESENTATION_ITEM ( '' )  );
#6578 = CONICAL_SURFACE ( 'NONE', #9227, 35.00000000000000711, 0.3490658503988666728 ) ;
#6580 = CARTESIAN_POINT ( 'NONE',  ( -30.90169943749474513, 27.70000000000000284, -42.53254041760200721 ) ) ;
#6581 = CARTESIAN_POINT ( 'NONE',  ( -15.45084971874736368, 24.40000000000000213, 47.55282581475768211 ) ) ;
#6582 = CARTESIAN_POINT ( 'NONE',  ( 17.35186893731097868, 20.17349094513210161, 101.0000000000000000 ) ) ;
#6583 = CARTESIAN_POINT ( 'NONE',  ( 50.00000000000000000, 48.78125000068279604, -6.123233995736766085E-15 ) ) ;
#6584 = CARTESIAN_POINT ( 'NONE',  ( 0.000000000000000000, 267.0000000000000000, 0.000000000000000000 ) ) ;
#6585 = CARTESIAN_POINT ( 'NONE',  ( 15.40903463028481113, 23.32187500034139660, -47.42413220539094709 ) ) ;
#6586 = SURFACE_STYLE_FILL_AREA ( #4165 ) ;
#6587 = LINE ( 'NONE', #13126, #3823 ) ;
#6588 = CARTESIAN_POINT ( 'NONE',  ( -49.99999999999999289, 37.88125000068279746, 16.24598481164533226 ) ) ;
#6589 = DIRECTION ( 'NONE',  ( 1.000000000000000000, 0.000000000000000000, 0.000000000000000000 ) ) ;
#6590 = EDGE_CURVE ( 'NONE', #12474, #761, #2541, .T. ) ;
#6591 = CARTESIAN_POINT ( 'NONE',  ( 15.45084971874736723, 23.40000000000000213, -47.55282581475768211 ) ) ;
#6592 = DIRECTION ( 'NONE',  ( 0.000000000000000000, -1.000000000000000000, 0.000000000000000000 ) ) ;
#6594 = ORIENTED_EDGE ( 'NONE', *, *, #915, .F. ) ;
#6593 = B_SPLINE_CURVE_WITH_KNOTS ( 'NONE', 3,
 ( #11982, #7916, #14385, #9412, #11817, #10588, #14222, #339, #6689, #3006, #423, #15801, #9500, #8167, #1517, #9166, #14547, #10418, #504, #5438, #8075, #6858, #3174, #11661, #11906, #10666, #15717, #14459, #6607, #3089, #10501, #1834, #5363, #15473, #2848, #12991, #1595, #5527, #4189, #9255, #14310, #2930, #7997, #13071, #7333, #8406, #2081, #14878, #9828, #14704, #3335, #7090, #14961, #4677, #13475, #1909, #834, #7003, #16048, #2159, #4589 ),
 .UNSPECIFIED., .F., .F.,
 ( 4, 3, 3, 3, 3, 3, 3, 3, 3, 3, 3, 3, 3, 3, 3, 3, 3, 3, 3, 3, 4 ),
 ( 0.000000000000000000, 0.0001250000981872742046, 0.0006250122739946097549, 0.001125024449802050283, 0.001625036625609320266, 0.002125048801416672649, 0.002625060977223844620, 0.003125073153031289810, 0.003625085328838455277, 0.004125097504645746510, 0.004625109680452854297, 0.005125121856260252649, 0.005625134032067359569, 0.006125146207874817769, 0.006625158383682326277, 0.007125170559489365542, 0.007625182735296597361, 0.008125194911103646167, 0.008625207086911106102, 0.009137502482429510006, 0.009649851960369987616 ),
 .UNSPECIFIED. ) ;
#6595 = CARTESIAN_POINT ( 'NONE',  ( 49.86468353125001585, 40.75937500034138594, 16.20201782572375038 ) ) ;
#6596 = ORIENTED_EDGE ( 'NONE', *, *, #1625, .T. ) ;
#6597 = FACE_OUTER_BOUND ( 'NONE', #14278, .T. ) ;
#6598 = DIRECTION ( 'NONE',  ( 1.000000000000000000, 0.000000000000000000, -0.000000000000000000 ) ) ;
#6599 = CARTESIAN_POINT ( 'NONE',  ( -30.81806926056963292, 29.55937500034139376, -42.41743335407647209 ) ) ;
#6600 = ORIENTED_EDGE ( 'NONE', *, *, #11297, .F. ) ;
#6601 = DIRECTION ( 'NONE',  ( -0.000000000000000000, 1.000000000000000000, -0.000000000000000000 ) ) ;
#6602 = CARTESIAN_POINT ( 'NONE',  ( -17.28056337048291269, 25.32136411938365583, 93.95934175966624480 ) ) ;
#6603 = DIRECTION ( 'NONE',  ( 0.8660254037844362651, 0.5000000000000041078, 0.000000000000000000 ) ) ;
#6604 = CARTESIAN_POINT ( 'NONE',  ( -30.81806926056963292, 33.62187500034139731, -42.41743335407646498 ) ) ;
#6605 = LINE ( 'NONE', #12989, #2015 ) ;
#6606 = CARTESIAN_POINT ( 'NONE',  ( -15.40903463028481646, 21.45937500034139589, -47.42413220539093999 ) ) ;
#6607 = CARTESIAN_POINT ( 'NONE',  ( -47.13255506291579877, 20.00000000000000355, 16.27994764699678854 ) ) ;
#6608 = CARTESIAN_POINT ( 'NONE',  ( -40.34137639590981905, 27.72187500034139873, -29.30972558990011478 ) ) ;
#6609 = CARTESIAN_POINT ( 'NONE',  ( -4.320770838041405604, 30.97531352606679178, 101.0000000000000000 ) ) ;
#6610 = CARTESIAN_POINT ( 'NONE',  ( 15.45084971874736723, 31.39999999999999858, -47.55282581475768211 ) ) ;
#6611 = CARTESIAN_POINT ( 'NONE',  ( -30.81806926056963292, 29.55937500034139376, -42.41743335407647209 ) ) ;
#6612 = CARTESIAN_POINT ( 'NONE',  ( -30.81806926056962226, 34.22187500034139873, 42.41743335407647919 ) ) ;
#6613 = AXIS2_PLACEMENT_3D ( 'NONE', #13685, #12777, #1378 ) ;
#6614 = ORIENTED_EDGE ( 'NONE', *, *, #7560, .F. ) ;
#6615 = UNCERTAINTY_MEASURE_WITH_UNIT (LENGTH_MEASURE( 1.000000000000000082E-05 ), #12209, 'distance_accuracy_value', 'NONE');
#6616 = CARTESIAN_POINT ( 'NONE',  ( 49.86468353125000164, 38.85937500034139447, -6.106662507704105588E-15 ) ) ;
#6617 = EDGE_LOOP ( 'NONE', ( #3684, #469, #9794, #12943 ) ) ;
#6618 = LINE ( 'NONE', #7604, #7345 ) ;
#6619 = CARTESIAN_POINT ( 'NONE',  ( -15.40903463028480580, 46.25937500034140015, 47.42413220539094709 ) ) ;
#6620 = CARTESIAN_POINT ( 'NONE',  ( 7.732050807568878525, 22.50000000000000000, 102.0000000000000142 ) ) ;
#6621 = CARTESIAN_POINT ( 'NONE',  ( 40.34137639590981905, 26.72187500034139518, 29.30972558990010768 ) ) ;
#6622 = FACE_OUTER_BOUND ( 'NONE', #12492, .T. ) ;
#6623 = VECTOR ( 'NONE', #12881, 1000.000000000000000 ) ;
#6624 = CARTESIAN_POINT ( 'NONE',  ( -40.34137639590981195, 34.12187500034139731, 29.30972558990012189 ) ) ;
#6625 = CARTESIAN_POINT ( 'NONE',  ( 49.86468353124999453, 44.95937500034139589, -16.20201782572376104 ) ) ;
#6626 = CARTESIAN_POINT ( 'NONE',  ( -3.111920190527341144E-15, 25.28125000068279604, -50.00000000000000000 ) ) ;
#6627 =( BOUNDED_CURVE ( )  B_SPLINE_CURVE ( 2, ( #4164, #9474, #6831, #1650, #10643, #15695, #15531, #11959, #7059, #636, #1814, #9233, #7976 ),
 .UNSPECIFIED., .F., .F. ) 
 B_SPLINE_CURVE_WITH_KNOTS ( ( 3, 2, 2, 2, 2, 2, 3 ),
 ( 0.1166666666666666685, 0.1199999999999999956, 0.1266666666666666774, 0.1333333333333333315, 0.1400000000000000133, 0.1466666666666666674, 0.1499999999999999944 ),
 .UNSPECIFIED. ) 
 CURVE ( )  GEOMETRIC_REPRESENTATION_ITEM ( )  RATIONAL_B_SPLINE_CURVE ( ( 0.9755282581475768211, 0.9755282581475768211, 1.000000000000000000, 0.9510565162951535312, 1.000000000000000000, 0.9510565162951535312, 1.000000000000000000, 0.9510565162951535312, 1.000000000000000000, 0.9510565162951535312, 1.000000000000000000, 0.9755282581475768211, 0.9755282581475768211 ) ) 
 REPRESENTATION_ITEM ( '' )  );
#6628 = EDGE_CURVE ( 'NONE', #8437, #3904, #6930, .T. ) ;
#6629 = CARTESIAN_POINT ( 'NONE',  ( 30.90169943749475578, 38.70000000000000284, 42.53254041760200010 ) ) ;
#6630 = CARTESIAN_POINT ( 'NONE',  ( -15.45084971874736368, 24.18125000068279817, 47.55282581475768211 ) ) ;
#6631 = CARTESIAN_POINT ( 'NONE',  ( 16.40338228813142507, 28.62403330670708002, 93.52543394180021608 ) ) ;
#6632 = CARTESIAN_POINT ( 'NONE',  ( -49.86468353125000164, 27.92187500034139447, 0.000000000000000000 ) ) ;
#6633 = EDGE_CURVE ( 'NONE', #9602, #1101, #579, .T. ) ;
#6634 = EDGE_CURVE ( 'NONE', #11447, #2664, #6772, .T. ) ;
#6635 = VECTOR ( 'NONE', #11715, 1000.000000000000000 ) ;
#6636 = CARTESIAN_POINT ( 'NONE',  ( -8.660254037844415720, 37.00000000000001421, -4.999999999999952038 ) ) ;
#6637 = ORIENTED_EDGE ( 'NONE', *, *, #127, .T. ) ;
#6638 = CARTESIAN_POINT ( 'NONE',  ( 50.00000000000000711, 34.68125000068279462, 16.24598481164530739 ) ) ;
#6639 = VERTEX_POINT ( 'NONE', #5601 ) ;
#6640 = EDGE_CURVE ( 'NONE', #2321, #15727, #6593, .T. ) ;
#6641 = DIRECTION ( 'NONE',  ( 6.938893903907231459E-18, -1.000000000000000000, -5.551115123125782702E-17 ) ) ;
#6642 = CARTESIAN_POINT ( 'NONE',  ( -24.78626291527393377, 40.00000000000000711, -5.650101528493794767 ) ) ;
#6643 = CARTESIAN_POINT ( 'NONE',  ( -14.53285685708567421, 14.68680145065682474, 102.0000000000000142 ) ) ;
#6644 = CARTESIAN_POINT ( 'NONE',  ( -15.40903463028480580, 46.32187500034140015, 47.42413220539094709 ) ) ;
#6645 = CARTESIAN_POINT ( 'NONE',  ( 15.40903463028482356, 22.45937500034139589, 47.42413220539093999 ) ) ;
#6646 = DIRECTION ( 'NONE',  ( -0.000000000000000000, -1.000000000000000000, -0.000000000000000000 ) ) ;
#6647 = ADVANCED_FACE ( 'NONE', ( #16142 ), #3507, .F. ) ;
#6648 = CARTESIAN_POINT ( 'NONE',  ( -3.210462471511496205E-15, 41.42187500034139447, -52.43083105670540789 ) ) ;
#6649 = AXIS2_PLACEMENT_3D ( 'NONE', #728, #5730, #10880 ) ;
#6650 = CARTESIAN_POINT ( 'NONE',  ( 7.919222016226693306, 34.33250428222964246, 50.00000000000003553 ) ) ;
#6651 = CARTESIAN_POINT ( 'NONE',  ( 49.86468353125000164, 48.92187500034139447, -6.106662507704105588E-15 ) ) ;
#6652 = PLANE ( 'NONE',  #11484 ) ;
#6653 = ORIENTED_EDGE ( 'NONE', *, *, #10082, .T. ) ;
#6654 = CARTESIAN_POINT ( 'NONE',  ( 49.86468353125001585, 46.82187500034139305, 16.20201782572375038 ) ) ;
#6655 = EDGE_LOOP ( 'NONE', ( #12711, #2859, #11060, #133 ) ) ;
#6656 = CARTESIAN_POINT ( 'NONE',  ( -0.4999999999999998890, 39.32590460608501104, 101.6666710454654208 ) ) ;
#6657 = VERTEX_POINT ( 'NONE', #3427 ) ;
#6658 = ORIENTED_EDGE ( 'NONE', *, *, #3489, .T. ) ;
#6659 = DIRECTION ( 'NONE',  ( 1.000000000000000000, 0.000000000000000000, 0.000000000000000000 ) ) ;
#6660 = LINE ( 'NONE', #14280, #4673 ) ;
#6661 = CARTESIAN_POINT ( 'NONE',  ( 40.45084971874737789, 28.80000000000000426, 29.38926261462365375 ) ) ;
#6662 = CARTESIAN_POINT ( 'NONE',  ( 9.657523855033129090E-15, 26.50000000000000355, 52.57311121191334990 ) ) ;
#6663 = CARTESIAN_POINT ( 'NONE',  ( 30.81806926056962936, 43.15937500034140584, -42.41743335407647209 ) ) ;
#6664 = DIRECTION ( 'NONE',  ( -0.8660254037844363761, 0.000000000000000000, 0.5000000000000041078 ) ) ;
#6665 = CARTESIAN_POINT ( 'NONE',  ( -7.732050807568878525, 22.50000000000000000, 102.0000000000000142 ) ) ;
#6666 = CARTESIAN_POINT ( 'NONE',  ( -3.210462471511496205E-15, 21.42187500034139802, -52.43083105670540789 ) ) ;
#6667 = SHAPE_REPRESENTATION_RELATIONSHIP ( 'NONE' , 'NONE' ,  #15095, #11759 ) ;
#6668 = APPLICATION_CONTEXT ( 'automotive_design' ) ;
#6669 = CARTESIAN_POINT ( 'NONE',  ( -3.111920190527341144E-15, 27.28125000068279604, -50.00000000000000000 ) ) ;
#6670 = CARTESIAN_POINT ( 'NONE',  ( 50.00000000000000711, 42.68125000068280173, 16.24598481164530739 ) ) ;
#6671 = LINE ( 'NONE', #5267, #14502 ) ;
#6672 = CARTESIAN_POINT ( 'NONE',  ( 15.45084971874736723, 21.18125000068279817, -47.55282581475768211 ) ) ;
#6673 = CARTESIAN_POINT ( 'NONE',  ( 0.000000000000000000, 193.4213562373095385, -50.00000000000000000 ) ) ;
#6674 = VERTEX_POINT ( 'NONE', #1993 ) ;
#6675 = CARTESIAN_POINT ( 'NONE',  ( 15.40903463028481113, 39.25937500034140015, -47.42413220539094709 ) ) ;
#6676 = ORIENTED_EDGE ( 'NONE', *, *, #14174, .F. ) ;
#6677 = CARTESIAN_POINT ( 'NONE',  ( -50.00000000000000000, 49.78125000068280315, 0.000000000000000000 ) ) ;
#6678 = CARTESIAN_POINT ( 'NONE',  ( 0.000000000000000000, 22.50000000000000000, 101.0000000000000000 ) ) ;
#6679 = CARTESIAN_POINT ( 'NONE',  ( 30.81806926056964002, 20.55937500034139376, 42.41743335407647209 ) ) ;
#6680 = ORIENTED_EDGE ( 'NONE', *, *, #16366, .T. ) ;
#6681 = PRODUCT ( 'cutter assembly', 'cutter assembly', '', ( #14349 ) ) ;
#6682 = EDGE_CURVE ( 'NONE', #9526, #11778, #8076, .T. ) ;
#6683 = DIRECTION ( 'NONE',  ( -0.000000000000000000, 1.000000000000000000, -0.000000000000000000 ) ) ;
#6684 = CARTESIAN_POINT ( 'NONE',  ( 22.35235477796485171, 99.04060251627520017, -4.999999999999976019 ) ) ;
#6685 = DIRECTION ( 'NONE',  ( 0.000000000000000000, 0.000000000000000000, -1.000000000000000000 ) ) ;
#6686 = CARTESIAN_POINT ( 'NONE',  ( -49.86468353124999453, 28.02187500034139589, 16.20201782572377169 ) ) ;
#6687 = CARTESIAN_POINT ( 'NONE',  ( -7.919222016226870942, 38.22999571913595673, 49.99999999999997158 ) ) ;
#6688 = CARTESIAN_POINT ( 'NONE',  ( 17.35865297518751049, 20.20728047528196925, 94.86179832180087601 ) ) ;
#6689 = CARTESIAN_POINT ( 'NONE',  ( -48.11476475577501333, 20.00000000000000355, 13.09518440665035754 ) ) ;
#6690 = CARTESIAN_POINT ( 'NONE',  ( -3.210462471511496205E-15, 27.42187500034139092, -52.43083105670540789 ) ) ;
#6691 = LINE ( 'NONE', #11739, #1772 ) ;
#6692 = CARTESIAN_POINT ( 'NONE',  ( -40.45084971874737789, 37.79999999999999716, -29.38926261462365730 ) ) ;
#6693 = CARTESIAN_POINT ( 'NONE',  ( -30.81806926056963292, 31.55937500034139731, -42.41743335407647209 ) ) ;
#6694 = CARTESIAN_POINT ( 'NONE',  ( 40.34137639590981195, 27.12187500034139731, -29.30972558990011834 ) ) ;
#6695 = CYLINDRICAL_SURFACE ( 'NONE', #3274, 17.50000000000000000 ) ;
#6696 = ORIENTED_EDGE ( 'NONE', *, *, #4491, .F. ) ;
#6697 = CARTESIAN_POINT ( 'NONE',  ( 15.40903463028482356, 32.45937500034138878, 47.42413220539093999 ) ) ;
#6698 = VERTEX_POINT ( 'NONE', #5759 ) ;
#6699 = CARTESIAN_POINT ( 'NONE',  ( 2.500000000000000000, 242.0000000000000284, -40.00000000000000000 ) ) ;
#6700 = CARTESIAN_POINT ( 'NONE',  ( -15.40903463028481646, 41.45937500034140299, -47.42413220539093999 ) ) ;
#6701 = CARTESIAN_POINT ( 'NONE',  ( -49.99999999999999289, 37.90000000000000568, -16.24598481164531449 ) ) ;
#6702 = CARTESIAN_POINT ( 'NONE',  ( 24.78235906514067111, 286.0218276482190731, 7.282359065130366460 ) ) ;
#6703 = CARTESIAN_POINT ( 'NONE',  ( -30.00000000000000711, 282.0000000000000000, 12.50000000000000000 ) ) ;
#6704 = CARTESIAN_POINT ( 'NONE',  ( -49.86468353125000164, 33.92187500034139447, 0.000000000000000000 ) ) ;
#6705 = CARTESIAN_POINT ( 'NONE',  ( -3.210462471511496205E-15, 37.35937500034140157, -52.43083105670540789 ) ) ;
#6706 = CYLINDRICAL_SURFACE ( 'NONE', #2812, 5.000000000000000000 ) ;
#6707 = CARTESIAN_POINT ( 'NONE',  ( -49.99999999999999289, 38.10000000000000142, 16.24598481164533226 ) ) ;
#6708 = CARTESIAN_POINT ( 'NONE',  ( 40.34137639590981195, 49.05937500034139731, -29.30972558990011834 ) ) ;
#6709 = CARTESIAN_POINT ( 'NONE',  ( -40.34137639590981905, 45.72187500034139873, -29.30972558990011478 ) ) ;
#6710 = EDGE_CURVE ( 'NONE', #305, #11087, #3509, .T. ) ;
#6711 = CARTESIAN_POINT ( 'NONE',  ( 40.34137639590981905, 28.72187500034139873, 29.30972558990010768 ) ) ;
#6712 = EDGE_CURVE ( 'NONE', #9704, #1226, #9580, .T. ) ;
#6713 = CARTESIAN_POINT ( 'NONE',  ( -40.34137639590981905, 47.65937500034139873, -29.30972558990011478 ) ) ;
#6714 = ORIENTED_EDGE ( 'NONE', *, *, #6634, .F. ) ;
#6715 = CARTESIAN_POINT ( 'NONE',  ( -15.45084971874736368, 34.18125000068279462, 47.55282581475768211 ) ) ;
#6716 = ORIENTED_EDGE ( 'NONE', *, *, #14306, .T. ) ;
#6717 = LINE ( 'NONE', #15503, #6015 ) ;
#6718 = LINE ( 'NONE', #7950, #1990 ) ;
#6719 = VECTOR ( 'NONE', #15781, 999.9999999999998863 ) ;
#6720 = CARTESIAN_POINT ( 'NONE',  ( -2.547328955960238000E-13, 32.28125000068278894, 49.99999999999999289 ) ) ;
#6721 = CARTESIAN_POINT ( 'NONE',  ( -40.34137639590981905, 47.72187500034139873, -29.30972558990011478 ) ) ;
#6722 = CARTESIAN_POINT ( 'NONE',  ( -40.34137639590981905, 25.65937500034139518, -29.30972558990011478 ) ) ;
#6723 = ADVANCED_FACE ( 'NONE', ( #6006 ), #12046, .T. ) ;
#6724 = PRODUCT_RELATED_PRODUCT_CATEGORY ( 'part', '', ( #6681 ) ) ;
#6725 = FACE_OUTER_BOUND ( 'NONE', #10344, .T. ) ;
#6726 = CARTESIAN_POINT ( 'NONE',  ( 49.86468353125001585, 40.82187500034140726, 16.20201782572375038 ) ) ;
#6727 = PRODUCT_CONTEXT ( 'NONE', #2490, 'mechanical' ) ;
#6728 = CARTESIAN_POINT ( 'NONE',  ( 0.000000000000000000, 193.4213562373095385, 0.000000000000000000 ) ) ;
#6729 = CARTESIAN_POINT ( 'NONE',  ( 30.81806926056962936, 45.22187500034139873, -42.41743335407647209 ) ) ;
#6730 = LINE ( 'NONE', #4054, #10693 ) ;
#6731 = VERTEX_POINT ( 'NONE', #11074 ) ;
#6732 = AXIS2_PLACEMENT_3D ( 'NONE', #8002, #13076, #10594 ) ;
#6733 = CARTESIAN_POINT ( 'NONE',  ( -30.81806926056963292, 45.62187500034139020, -42.41743335407647209 ) ) ;
#6734 = B_SPLINE_CURVE_WITH_KNOTS ( 'NONE', 3,
 ( #6016, #2249, #2166, #7260 ),
 .UNSPECIFIED., .F., .F.,
 ( 4, 4 ),
 ( 2.829004760673572825E-07, 0.001414802801989366570 ),
 .UNSPECIFIED. ) ;
#6735 = VERTEX_POINT ( 'NONE', #2241 ) ;
#6736 = CARTESIAN_POINT ( 'NONE',  ( -30.90169943749473447, 26.29999999999999716, 42.53254041760200721 ) ) ;
#6737 = VERTEX_POINT ( 'NONE', #9907 ) ;
#6738 = ORIENTED_EDGE ( 'NONE', *, *, #10776, .T. ) ;
#6739 = ADVANCED_FACE ( 'NONE', ( #662 ), #14593, .T. ) ;
#6740 = CARTESIAN_POINT ( 'NONE',  ( -30.90169943749474513, 43.48125000068279178, -42.53254041760200721 ) ) ;
#6741 = CARTESIAN_POINT ( 'NONE',  ( 50.00000000000000000, 38.78125000068279604, -6.123233995736766085E-15 ) ) ;
#6742 = CARTESIAN_POINT ( 'NONE',  ( 6.123233995736766085E-15, 193.4213562373095385, 50.00000000000000000 ) ) ;
#6743 = CARTESIAN_POINT ( 'NONE',  ( 30.90169943749475578, 24.69999999999999929, 42.53254041760200010 ) ) ;
#6744 = CARTESIAN_POINT ( 'NONE',  ( -3.210462471511496205E-15, 41.35937500034138736, -52.43083105670540789 ) ) ;
#6745 = CARTESIAN_POINT ( 'NONE',  ( -30.90169943749474513, 25.48125000068279888, -42.53254041760200721 ) ) ;
#6746 = DIRECTION ( 'NONE',  ( 0.000000000000000000, -0.000000000000000000, 1.000000000000000000 ) ) ;
#6747 = AXIS2_PLACEMENT_3D ( 'NONE', #11733, #335, #5434 ) ;
#6748 = DIRECTION ( 'NONE',  ( 0.000000000000000000, 0.000000000000000000, -1.000000000000000000 ) ) ;
#6749 = EDGE_CURVE ( 'NONE', #15727, #12890, #1994, .T. ) ;
#6750 =( NAMED_UNIT ( * ) PLANE_ANGLE_UNIT ( ) SI_UNIT ( $, .RADIAN. ) );
#6751 = FACE_OUTER_BOUND ( 'NONE', #10386, .T. ) ;
#6752 = CARTESIAN_POINT ( 'NONE',  ( 50.00000000000000711, 40.68125000068280173, 16.24598481164530739 ) ) ;
#6753 = LINE ( 'NONE', #3996, #12405 ) ;
#6754 = EDGE_CURVE ( 'NONE', #15993, #5627, #15968, .T. ) ;
#6755 = CARTESIAN_POINT ( 'NONE',  ( -8.477241335952138357, 18.18301270189218855, 101.0000000000000000 ) ) ;
#6756 = CARTESIAN_POINT ( 'NONE',  ( -16.45433951800529826, 21.27333336793995144, 102.0000000000000142 ) ) ;
#6757 = EDGE_LOOP ( 'NONE', ( #8083, #877, #8793, #10480, #6939 ) ) ;
#6758 = CARTESIAN_POINT ( 'NONE',  ( -49.86468353124999453, 35.75937500034140015, -16.20201782572375393 ) ) ;
#6759 = ORIENTED_EDGE ( 'NONE', *, *, #14415, .T. ) ;
#6760 = ORIENTED_EDGE ( 'NONE', *, *, #7347, .T. ) ;
#6761 = VECTOR ( 'NONE', #6090, 1000.000000000000000 ) ;
#6762 = CARTESIAN_POINT ( 'NONE',  ( 49.99999999999999289, 46.88125000068279036, -16.24598481164532160 ) ) ;
#6763 = CARTESIAN_POINT ( 'NONE',  ( 0.000000000000000000, 25.00000000000000355, 0.000000000000000000 ) ) ;
#6764 = CARTESIAN_POINT ( 'NONE',  ( 9.631387414534489405E-15, 22.35937500034139802, 52.43083105670540789 ) ) ;
#6765 = ORIENTED_EDGE ( 'NONE', *, *, #5989, .T. ) ;
#6766 = CARTESIAN_POINT ( 'NONE',  ( -8.487905985326070990, 95.47132599478250370, -3.471325994782474389 ) ) ;
#6767 = DIRECTION ( 'NONE',  ( 1.000000000000000000, -0.000000000000000000, 1.224646799147353207E-16 ) ) ;
#6768 = DIRECTION ( 'NONE',  ( -0.000000000000000000, -1.000000000000000000, -0.000000000000000000 ) ) ;
#6769 = CARTESIAN_POINT ( 'NONE',  ( 15.40903463028481113, 29.32187500034139660, -47.42413220539094709 ) ) ;
#6770 = CARTESIAN_POINT ( 'NONE',  ( 7.732050807568878525, 22.50000000000000000, 100.0000000000000000 ) ) ;
#6771 = CARTESIAN_POINT ( 'NONE',  ( 0.000000000000000000, 28.00000000000000355, 0.000000000000000000 ) ) ;
#6772 = LINE ( 'NONE', #1674, #14693 ) ;
#6773 = ADVANCED_FACE ( 'NONE', ( #1320 ), #10230, .F. ) ;
#6774 = CARTESIAN_POINT ( 'NONE',  ( -30.81806926056962226, 30.22187500034139518, 42.41743335407647209 ) ) ;
#6775 = DIRECTION ( 'NONE',  ( 0.000000000000000000, 0.000000000000000000, -1.000000000000000000 ) ) ;
#6776 = VECTOR ( 'NONE', #13854, 1000.000000000000000 ) ;
#6777 = CARTESIAN_POINT ( 'NONE',  ( -40.45084971874737079, 36.20000000000000284, 29.38926261462367151 ) ) ;
#6778 = CARTESIAN_POINT ( 'NONE',  ( 30.81806926056964002, 32.55937500034139731, 42.41743335407647209 ) ) ;
#6779 = LINE ( 'NONE', #11912, #10445 ) ;
#6780 = ORIENTED_EDGE ( 'NONE', *, *, #9277, .F. ) ;
#6781 = CARTESIAN_POINT ( 'NONE',  ( -49.86468353124999453, 29.95937500034139589, 16.20201782572377169 ) ) ;
#6782 = ORIENTED_EDGE ( 'NONE', *, *, #3477, .T. ) ;
#6783 = CARTESIAN_POINT ( 'NONE',  ( 20.00000000000000000, 307.0000000000000568, 7.500000000000002665 ) ) ;
#6784 = CARTESIAN_POINT ( 'NONE',  ( -15.40903463028480580, 42.25937500034139305, 47.42413220539094709 ) ) ;
#6785 = VECTOR ( 'NONE', #3416, 1000.000000000000000 ) ;
#6786 = DIRECTION ( 'NONE',  ( -0.9777979793268661846, 0.2095497831645198317, 0.000000000000000000 ) ) ;
#6787 = CARTESIAN_POINT ( 'NONE',  ( 15.40903463028482356, 20.52187500034139589, 47.42413220539093999 ) ) ;
#6788 = CARTESIAN_POINT ( 'NONE',  ( -24.86904120090709469, 286.8604097559688739, 7.369041200906232270 ) ) ;
#6789 = CARTESIAN_POINT ( 'NONE',  ( -15.40903463028481646, 35.52187500034139589, -47.42413220539093999 ) ) ;
#6790 = CARTESIAN_POINT ( 'NONE',  ( -49.86468353124999453, 37.75937500034140015, -16.20201782572375393 ) ) ;
#6791 = CARTESIAN_POINT ( 'NONE',  ( -9.289494224341229511, 8.863457290943159705, 102.0000000000000142 ) ) ;
#6792 = CARTESIAN_POINT ( 'NONE',  ( 15.45084971874736723, 43.39999999999999858, -47.55282581475768211 ) ) ;
#6793 = CARTESIAN_POINT ( 'NONE',  ( 15.45084971874737789, 22.38125000068280102, 47.55282581475767500 ) ) ;
#6794 = CARTESIAN_POINT ( 'NONE',  ( 40.34137639590981905, 46.72187500034139873, 29.30972558990010768 ) ) ;
#6795 = COLOUR_RGB ( '', 0.72549020, 0.75294118, 0.79215686) ;
#6796 = CARTESIAN_POINT ( 'NONE',  ( -15.40903463028481646, 27.52187500034139944, -47.42413220539093999 ) ) ;
#6797 = CARTESIAN_POINT ( 'NONE',  ( -40.45084971874737079, 27.98125000068279888, 29.38926261462367151 ) ) ;
#6798 = ORIENTED_EDGE ( 'NONE', *, *, #12723, .F. ) ;
#6799 = CARTESIAN_POINT ( 'NONE',  ( -49.99999999999999289, 31.68125000068279462, -16.24598481164531449 ) ) ;
#6800 = ORIENTED_EDGE ( 'NONE', *, *, #14844, .F. ) ;
#6801 = CARTESIAN_POINT ( 'NONE',  ( 0.000000000000000000, 267.0000000000000000, -40.00000000000000000 ) ) ;
#6802 = CYLINDRICAL_SURFACE ( 'NONE', #10525, 45.00000000000000711 ) ;
#6803 = VECTOR ( 'NONE', #8371, 1000.000000000000114 ) ;
#6804 = CARTESIAN_POINT ( 'NONE',  ( 49.99999999999999289, 30.88125000068279746, -16.24598481164532160 ) ) ;
#6805 = CARTESIAN_POINT ( 'NONE',  ( 40.34137639590981195, 47.12187500034140442, -29.30972558990011834 ) ) ;
#6806 = CARTESIAN_POINT ( 'NONE',  ( 30.81806926056964002, 24.55937500034139376, 42.41743335407647209 ) ) ;
#6807 = DIRECTION ( 'NONE',  ( 0.000000000000000000, 1.000000000000000000, 0.000000000000000000 ) ) ;
#6808 = CARTESIAN_POINT ( 'NONE',  ( 49.86468353125001585, 38.82187500034140015, 16.20201782572375038 ) ) ;
#6809 = SHAPE_DEFINITION_REPRESENTATION ( #1335, #5560 ) ;
#6810 = CARTESIAN_POINT ( 'NONE',  ( 9.631387414534489405E-15, 48.42187500034140157, 52.43083105670540789 ) ) ;
#6811 = CARTESIAN_POINT ( 'NONE',  ( 49.99999999999999289, 31.09999999999999787, -16.24598481164532160 ) ) ;
#6812 = CIRCLE ( 'NONE', #10522, 16.50000000000000711 ) ;
#6813 = AXIS2_PLACEMENT_3D ( 'NONE', #15962, #827, #13790 ) ;
#6814 = EDGE_LOOP ( 'NONE', ( #5349, #12275, #13461, #3236 ) ) ;
#6815 = AXIS2_PLACEMENT_3D ( 'NONE', #1548, #6883, #7786 ) ;
#6816 = AXIS2_PLACEMENT_3D ( 'NONE', #4136, #6646, #12400 ) ;
#6817 = CARTESIAN_POINT ( 'NONE',  ( -40.34137639590981195, 20.05937500034139731, 29.30972558990012189 ) ) ;
#6818 = VERTEX_POINT ( 'NONE', #7487 ) ;
#6819 = EDGE_LOOP ( 'NONE', ( #15461, #5970, #6714, #13681 ) ) ;
#6820 =( BOUNDED_CURVE ( )  B_SPLINE_CURVE ( 2, ( #7505, #15312, #13893, #12576, #2509, #4953, #2428, #7588, #3933, #7832, #10013, #8915, #9004 ),
 .UNSPECIFIED., .F., .F. ) 
 B_SPLINE_CURVE_WITH_KNOTS ( ( 3, 2, 2, 2, 2, 2, 3 ),
 ( 0.2166666666666666741, 0.2200000000000000011, 0.2266666666666666552, 0.2333333333333333370, 0.2399999999999999911, 0.2466666666666666730, 0.2500000000000000000 ),
 .UNSPECIFIED. ) 
 CURVE ( )  GEOMETRIC_REPRESENTATION_ITEM ( )  RATIONAL_B_SPLINE_CURVE ( ( 0.9755282581475768211, 0.9755282581475768211, 1.000000000000000000, 0.9510565162951535312, 1.000000000000000000, 0.9510565162951535312, 1.000000000000000000, 0.9510565162951535312, 1.000000000000000000, 0.9510565162951535312, 1.000000000000000000, 0.9755282581475768211, 0.9755282581475765991 ) ) 
 REPRESENTATION_ITEM ( '' )  );
#6821 = DIRECTION ( 'NONE',  ( -0.3090169943749574988, 0.9510565162951503115, 0.000000000000000000 ) ) ;
#6822 = LINE ( 'NONE', #10560, #2532 ) ;
#6823 = LINE ( 'NONE', #7054, #3342 ) ;
#6824 = CARTESIAN_POINT ( 'NONE',  ( -50.00000000000000000, 26.00000000000000355, 0.000000000000000000 ) ) ;
#6825 = AXIS2_PLACEMENT_3D ( 'NONE', #12870, #6479, #227 ) ;
#6826 = CARTESIAN_POINT ( 'NONE',  ( 30.81806926056964002, 46.55937500034139020, 42.41743335407647209 ) ) ;
#6827 = CIRCLE ( 'NONE', #8392, 16.50000000000000711 ) ;
#6828 = CIRCLE ( 'NONE', #15837, 2.000000000000001776 ) ;
#6829 = CARTESIAN_POINT ( 'NONE',  ( 49.99999999999999289, 48.88125000068280457, -16.24598481164532160 ) ) ;
#6830 = CARTESIAN_POINT ( 'NONE',  ( -7.499999999999998224, 40.00000000000000711, -24.29058411375428150 ) ) ;
#6831 = CARTESIAN_POINT ( 'NONE',  ( -15.45084971874736368, 46.40000000000000568, 47.55282581475768211 ) ) ;
#6832 = CARTESIAN_POINT ( 'NONE',  ( 49.99999999999999289, 49.10000000000000142, -16.24598481164532160 ) ) ;
#6833 = CARTESIAN_POINT ( 'NONE',  ( 40.45084971874737079, 32.98125000068279888, -29.38926261462366440 ) ) ;
#6834 = CARTESIAN_POINT ( 'NONE',  ( -49.99999999999999289, 37.68125000068279462, -16.24598481164531449 ) ) ;
#6835 = ADVANCED_FACE ( 'NONE', ( #8731 ), #16296, .T. ) ;
#6836 = CARTESIAN_POINT ( 'NONE',  ( 2.600676159226420495E-13, 21.28125000068279604, -49.99999999999999289 ) ) ;
#6837 = DIRECTION ( 'NONE',  ( 0.000000000000000000, 0.000000000000000000, -1.000000000000000000 ) ) ;
#6838 = ORIENTED_EDGE ( 'NONE', *, *, #14308, .T. ) ;
#6839 = CARTESIAN_POINT ( 'NONE',  ( -15.40903463028480580, 40.25937500034139305, 47.42413220539094709 ) ) ;
#6840 = ORIENTED_EDGE ( 'NONE', *, *, #5021, .F. ) ;
#6841 = ORIENTED_EDGE ( 'NONE', *, *, #2331, .T. ) ;
#6843 = ADVANCED_FACE ( 'NONE', ( #13957 ), #5955, .T. ) ;
#6842 = VECTOR ( 'NONE', #13061, 1000.000000000000000 ) ;
#6844 = EDGE_CURVE ( 'NONE', #1788, #6342, #528, .T. ) ;
#6845 = CARTESIAN_POINT ( 'NONE',  ( 50.00000000000000711, 42.89999999999999147, 16.24598481164530739 ) ) ;
#6846 = DIRECTION ( 'NONE',  ( 0.8660254037844326014, 0.000000000000000000, -0.5000000000000104361 ) ) ;
#6847 = CARTESIAN_POINT ( 'NONE',  ( 30.81806926056962936, 21.15937500034140228, -42.41743335407647209 ) ) ;
#6848 = EDGE_LOOP ( 'NONE', ( #14452, #15878, #14971, #14513 ) ) ;
#6849 = EDGE_CURVE ( 'NONE', #14942, #1352, #2409, .T. ) ;
#6850 = CARTESIAN_POINT ( 'NONE',  ( -50.00000000000000000, 20.00000000000000000, 0.000000000000000000 ) ) ;
#6851 = FACE_OUTER_BOUND ( 'NONE', #3125, .T. ) ;
#6852 = CARTESIAN_POINT ( 'NONE',  ( 19.99999999999999645, 307.0000000000000568, -2.499999999999999556 ) ) ;
#6853 = CARTESIAN_POINT ( 'NONE',  ( -15.40903463028481646, 25.52187500034139589, -47.42413220539093999 ) ) ;
#6854 = LINE ( 'NONE', #11904, #9997 ) ;
#6855 = B_SPLINE_CURVE_WITH_KNOTS ( 'NONE', 3,
 ( #15279, #16378, #10312, #7727 ),
 .UNSPECIFIED., .F., .F.,
 ( 4, 4 ),
 ( 2.829004760695596740E-07, 0.001414802801989369606 ),
 .UNSPECIFIED. ) ;
#6856 = VECTOR ( 'NONE', #14627, 1000.000000000000227 ) ;
#6857 = DIRECTION ( 'NONE',  ( 0.000000000000000000, 0.000000000000000000, 1.000000000000000000 ) ) ;
#6858 = CARTESIAN_POINT ( 'NONE',  ( -47.50025713571316999, 20.00000000000001066, 15.17274647889583861 ) ) ;
#6859 = CARTESIAN_POINT ( 'NONE',  ( -49.86468353125000164, 23.92187500034139447, 0.000000000000000000 ) ) ;
#6860 = AXIS2_PLACEMENT_3D ( 'NONE', #6898, #11952, #9381 ) ;
#6861 = DIRECTION ( 'NONE',  ( 0.000000000000000000, 0.000000000000000000, 1.000000000000000000 ) ) ;
#6862 = CARTESIAN_POINT ( 'NONE',  ( 40.45084971874737079, 33.20000000000000284, -29.38926261462366440 ) ) ;
#6863 = CARTESIAN_POINT ( 'NONE',  ( -49.86468353125000164, 33.85937500034139447, 0.000000000000000000 ) ) ;
#6864 = CARTESIAN_POINT ( 'NONE',  ( 15.45084971874736723, 39.40000000000000568, -47.55282581475768211 ) ) ;
#6865 = ORIENTED_EDGE ( 'NONE', *, *, #5330, .T. ) ;
#6866 = CARTESIAN_POINT ( 'NONE',  ( 40.34137639590981195, 31.05937500034139731, -29.30972558990011834 ) ) ;
#6867 = ORIENTED_EDGE ( 'NONE', *, *, #9014, .T. ) ;
#6868 = CARTESIAN_POINT ( 'NONE',  ( -3.147895402235901141, 5.285449336779595164, 101.0000000000000000 ) ) ;
#6869 = CARTESIAN_POINT ( 'NONE',  ( 49.86468353124999453, 42.95937500034139589, -16.20201782572376459 ) ) ;
#6870 = CARTESIAN_POINT ( 'NONE',  ( 29.34550962211229930, 282.0322304394513253, 11.19101924422353811 ) ) ;
#6871 = CARTESIAN_POINT ( 'NONE',  ( -15.40903463028480580, 38.32187500034140015, 47.42413220539094709 ) ) ;
#6872 = CARTESIAN_POINT ( 'NONE',  ( 49.86468353125001585, 38.75937500034139305, 16.20201782572375038 ) ) ;
#6873 = LINE ( 'NONE', #11924, #14472 ) ;
#6874 = CARTESIAN_POINT ( 'NONE',  ( 15.45084971874736723, 41.40000000000000568, -47.55282581475768211 ) ) ;
#6875 = CARTESIAN_POINT ( 'NONE',  ( -15.45084971874737256, 23.38125000068280102, -47.55282581475767500 ) ) ;
#6876 = CARTESIAN_POINT ( 'NONE',  ( -40.34137639590981195, 44.12187500034139731, 29.30972558990012189 ) ) ;
#6877 = CARTESIAN_POINT ( 'NONE',  ( -15.40903463028480580, 30.32187500034140015, 47.42413220539094709 ) ) ;
#6878 = CARTESIAN_POINT ( 'NONE',  ( -15.40903463028481646, 47.45937500034139589, -47.42413220539093999 ) ) ;
#6879 = EDGE_LOOP ( 'NONE', ( #15611, #14191, #13747, #11446 ) ) ;
#6880 = CARTESIAN_POINT ( 'NONE',  ( 40.45084971874737789, 32.58125000068280031, 29.38926261462365375 ) ) ;
#6881 = CIRCLE ( 'NONE', #16163, 17.50000000000000000 ) ;
#6882 = ORIENTED_EDGE ( 'NONE', *, *, #10785, .T. ) ;
#6883 = DIRECTION ( 'NONE',  ( 0.000000000000000000, 0.000000000000000000, -1.000000000000000000 ) ) ;
#6884 = CARTESIAN_POINT ( 'NONE',  ( 0.000000000000000000, 25.00000000000000000, 0.000000000000000000 ) ) ;
#6885 = CARTESIAN_POINT ( 'NONE',  ( 40.34137639590981905, 42.72187500034139873, 29.30972558990010768 ) ) ;
#6886 = EDGE_CURVE ( 'NONE', #5468, #9544, #5095, .T. ) ;
#6887 = CARTESIAN_POINT ( 'NONE',  ( 15.40903463028481113, 23.25937500034139660, -47.42413220539094709 ) ) ;
#6888 = CARTESIAN_POINT ( 'NONE',  ( 2.978552182361884590E-14, 47.50000000000000711, -50.00000000000000000 ) ) ;
#6889 = CARTESIAN_POINT ( 'NONE',  ( -40.34137639590981905, 39.72187500034139873, -29.30972558990011478 ) ) ;
#6890 = DIRECTION ( 'NONE',  ( 1.000000000000000000, 0.000000000000000000, 0.000000000000000000 ) ) ;
#6891 = CIRCLE ( 'NONE', #233, 79.49773270518484480 ) ;
#6892 = CARTESIAN_POINT ( 'NONE',  ( 9.631387414534489405E-15, 44.42187500034140157, 52.43083105670540789 ) ) ;
#6893 = DIRECTION ( 'NONE',  ( -0.5000000000000103251, 0.000000000000000000, -0.8660254037844327124 ) ) ;
#6894 = ORIENTED_EDGE ( 'NONE', *, *, #7286, .F. ) ;
#6895 = CARTESIAN_POINT ( 'NONE',  ( -30.81806926056963292, 43.62187500034139020, -42.41743335407647209 ) ) ;
#6896 = ORIENTED_EDGE ( 'NONE', *, *, #10486, .F. ) ;
#6897 = VERTEX_POINT ( 'NONE', #3914 ) ;
#6898 = CARTESIAN_POINT ( 'NONE',  ( 0.000000000000000000, 22.50000000000000000, 80.00000000000000000 ) ) ;
#6899 = CARTESIAN_POINT ( 'NONE',  ( 0.000000000000000000, 22.50000000000000000, 101.0000000000000000 ) ) ;
#6900 = CARTESIAN_POINT ( 'NONE',  ( 0.000000000000000000, 22.50000000000000000, 101.0000000000000000 ) ) ;
#6901 = CARTESIAN_POINT ( 'NONE',  ( 15.45084971874737789, 22.60000000000000142, 47.55282581475767500 ) ) ;
#6902 = VECTOR ( 'NONE', #1649, 1000.000000000000000 ) ;
#6903 = CARTESIAN_POINT ( 'NONE',  ( 40.34137639590981195, 41.05937500034139731, -29.30972558990011834 ) ) ;
#6904 = DIRECTION ( 'NONE',  ( 1.000000000000000000, 0.000000000000000000, 0.000000000000000000 ) ) ;
#6905 = DIRECTION ( 'NONE',  ( 0.000000000000000000, 0.000000000000000000, -1.000000000000000000 ) ) ;
#6906 = CARTESIAN_POINT ( 'NONE',  ( -7.919222016226688865, 33.33250428222964956, -50.00000000000003553 ) ) ;
#6907 = DIRECTION ( 'NONE',  ( 0.000000000000000000, 0.000000000000000000, -1.000000000000000000 ) ) ;
#6908 = CARTESIAN_POINT ( 'NONE',  ( 50.00000000000000711, 32.68125000068279462, 16.24598481164530739 ) ) ;
#6909 = DIRECTION ( 'NONE',  ( 0.000000000000000000, 1.000000000000000000, 0.000000000000000000 ) ) ;
#6910 = CARTESIAN_POINT ( 'NONE',  ( 7.919222016226875382, 37.44874571845315359, -49.99999999999997158 ) ) ;
#6911 = CARTESIAN_POINT ( 'NONE',  ( 1.293669679204937499E-13, 37.50000000000000711, -50.00000000000000000 ) ) ;
#6912 = ORIENTED_EDGE ( 'NONE', *, *, #8796, .T. ) ;
#6913 =( BOUNDED_CURVE ( )  B_SPLINE_CURVE ( 3, ( #3018, #13163, #2773, #10516 ),
 .UNSPECIFIED., .F., .F. ) 
 B_SPLINE_CURVE_WITH_KNOTS ( ( 4, 4 ),
 ( 1.570796326794896780, 3.141592653589793116 ),
 .UNSPECIFIED. ) 
 CURVE ( )  GEOMETRIC_REPRESENTATION_ITEM ( )  RATIONAL_B_SPLINE_CURVE ( ( 1.000000000000000000, 0.8047378541243650485, 0.8047378541243650485, 1.000000000000000000 ) ) 
 REPRESENTATION_ITEM ( '' )  );
#6914 = CARTESIAN_POINT ( 'NONE',  ( -40.34137639590981195, 32.05937500034139731, 29.30972558990012189 ) ) ;
#6915 = VECTOR ( 'NONE', #14360, 1000.000000000000000 ) ;
#6916 = VERTEX_POINT ( 'NONE', #12643 ) ;
#6917 = ORIENTED_EDGE ( 'NONE', *, *, #11253, .T. ) ;
#6918 = CARTESIAN_POINT ( 'NONE',  ( -3.111920190527341144E-15, 43.50000000000000711, -50.00000000000000000 ) ) ;
#6919 = LINE ( 'NONE', #328, #13195 ) ;
#6920 = CARTESIAN_POINT ( 'NONE',  ( -15.40903463028481646, 23.45937500034139944, -47.42413220539093999 ) ) ;
#6921 = ORIENTED_EDGE ( 'NONE', *, *, #6849, .T. ) ;
#6922 = CARTESIAN_POINT ( 'NONE',  ( -7.919222016226804328, 48.44874571845315359, 50.00000000000000000 ) ) ;
#6923 = CARTESIAN_POINT ( 'NONE',  ( 0.000000000000000000, 22.50000000000000000, 102.0000000000000142 ) ) ;
#6924 = DIRECTION ( 'NONE',  ( 0.8660254037844362651, -8.780190904559507395E-17, -0.5000000000000042188 ) ) ;
#6925 = CARTESIAN_POINT ( 'NONE',  ( 30.81806926056962936, 29.22187500034139873, -42.41743335407646498 ) ) ;
#6926 = CARTESIAN_POINT ( 'NONE',  ( -15.45084971874736368, 30.18125000068280173, 47.55282581475768211 ) ) ;
#6927 = CARTESIAN_POINT ( 'NONE',  ( 50.00000000000000711, 46.90000000000000568, 16.24598481164530739 ) ) ;
#6928 = ADVANCED_FACE ( 'NONE', ( #2658 ), #10467, .T. ) ;
#6929 = PRODUCT_DEFINITION ( 'UNKNOWN', '', #6018, #14712 ) ;
#6930 = LINE ( 'NONE', #4269, #3891 ) ;
#6931 = CARTESIAN_POINT ( 'NONE',  ( 30.81806926056964002, 22.62187500034139731, 42.41743335407646498 ) ) ;
#6932 = CARTESIAN_POINT ( 'NONE',  ( 4.898587196589413026E-15, 20.00000000000000355, 40.00000000000000000 ) ) ;
#6933 = CARTESIAN_POINT ( 'NONE',  ( -49.99999999999999289, 37.90000000000000568, -16.24598481164531449 ) ) ;
#6934 = CARTESIAN_POINT ( 'NONE',  ( -3.210462471511496205E-15, 27.35937500034139802, -52.43083105670540789 ) ) ;
#6935 = DIRECTION ( 'NONE',  ( -0.4999999999999917843, 0.000000000000000000, 0.8660254037844434816 ) ) ;
#6936 = EDGE_CURVE ( 'NONE', #6499, #2831, #7567, .T. ) ;
#6937 = EDGE_LOOP ( 'NONE', ( #5610, #14737 ) ) ;
#6938 = CARTESIAN_POINT ( 'NONE',  ( -40.34137639590981905, 27.65937500034139873, -29.30972558990011478 ) ) ;
#6939 = ORIENTED_EDGE ( 'NONE', *, *, #7286, .T. ) ;
#6940 = CARTESIAN_POINT ( 'NONE',  ( -48.98979485566356118, 261.9999999999999432, 10.00000000000000178 ) ) ;
#6941 = CARTESIAN_POINT ( 'NONE',  ( -49.86468353125000164, 39.85937500034139447, 0.000000000000000000 ) ) ;
#6942 = EDGE_CURVE ( 'NONE', #15954, #14909, #12047, .T. ) ;
#6943 = CARTESIAN_POINT ( 'NONE',  ( 25.48725218877856946, 284.2907069533055733, 7.987252188778913187 ) ) ;
#6944 = CARTESIAN_POINT ( 'NONE',  ( -29.34549410641294287, 282.0000000000000000, 12.17274705320727257 ) ) ;
#6945 = CARTESIAN_POINT ( 'NONE',  ( -40.34137639590981195, 32.12187500034140442, 29.30972558990012189 ) ) ;
#6946 = CARTESIAN_POINT ( 'NONE',  ( -15.40903463028480580, 34.25937500034139305, 47.42413220539094709 ) ) ;
#6947 = PLANE ( 'NONE',  #15273 ) ;
#6948 = CARTESIAN_POINT ( 'NONE',  ( -40.34137639590981195, 28.12187500034139731, 29.30972558990012189 ) ) ;
#6949 = CARTESIAN_POINT ( 'NONE',  ( -49.99999999999999289, 42.09999999999999432, 16.24598481164533226 ) ) ;
#6950 = CARTESIAN_POINT ( 'NONE',  ( 49.86468353125001585, 42.75937500034138594, 16.20201782572375038 ) ) ;
#6951 = CARTESIAN_POINT ( 'NONE',  ( 49.86468353125000164, 46.92187500034139447, -6.106662507704105588E-15 ) ) ;
#6952 = EDGE_CURVE ( 'NONE', #9016, #14534, #9989, .T. ) ;
#6953 = CARTESIAN_POINT ( 'NONE',  ( 15.45084971874736723, 49.39999999999999858, -47.55282581475768211 ) ) ;
#6954 = EDGE_LOOP ( 'NONE', ( #14572, #2478 ) ) ;
#6955 = CARTESIAN_POINT ( 'NONE',  ( -49.86468353124999453, 45.95937500034138878, 16.20201782572377169 ) ) ;
#6956 = ORIENTED_EDGE ( 'NONE', *, *, #11569, .T. ) ;
#6958 = EDGE_CURVE ( 'NONE', #4332, #11934, #14674, .T. ) ;
#6957 = CARTESIAN_POINT ( 'NONE',  ( 40.45084971874737079, 32.98125000068279888, -29.38926261462366440 ) ) ;
#6959 = ORIENTED_EDGE ( 'NONE', *, *, #4233, .T. ) ;
#6960 = PLANE ( 'NONE',  #413 ) ;
#6961 = CARTESIAN_POINT ( 'NONE',  ( -50.00000000000000000, 33.78125000068280315, 0.000000000000000000 ) ) ;
#6962 = CARTESIAN_POINT ( 'NONE',  ( -40.34137639590981905, 39.72187500034139873, -29.30972558990011478 ) ) ;
#6963 = CARTESIAN_POINT ( 'NONE',  ( 49.86468353125000164, 22.85937500034139802, -6.106662507704105588E-15 ) ) ;
#6964 = CARTESIAN_POINT ( 'NONE',  ( -0.4999999999999990563, 31.99999999999998579, 101.0000000000000000 ) ) ;
#6965 = PRODUCT_CONTEXT ( 'NONE', #14687, 'mechanical' ) ;
#6966 = CARTESIAN_POINT ( 'NONE',  ( 30.90169943749475578, 34.70000000000000995, 42.53254041760200010 ) ) ;
#6967 = EDGE_CURVE ( 'NONE', #14589, #7197, #13715, .T. ) ;
#6968 = CARTESIAN_POINT ( 'NONE',  ( -49.86468353124999453, 43.82187500034140015, -16.20201782572375393 ) ) ;
#6969 = DIRECTION ( 'NONE',  ( 0.000000000000000000, 1.000000000000000000, 0.000000000000000000 ) ) ;
#6970 = ORIENTED_EDGE ( 'NONE', *, *, #14631, .F. ) ;
#6971 = CARTESIAN_POINT ( 'NONE',  ( 49.86468353125000164, 40.92187500034139447, -6.106662507704105588E-15 ) ) ;
#6972 = EDGE_LOOP ( 'NONE', ( #13707, #7553, #1409, #3552 ) ) ;
#6973 = EDGE_LOOP ( 'NONE', ( #13097, #11501, #9708 ) ) ;
#6974 = DIRECTION ( 'NONE',  ( 0.000000000000000000, 1.000000000000000000, 0.000000000000000000 ) ) ;
#6975 = DIRECTION ( 'NONE',  ( 0.000000000000000000, 0.000000000000000000, -1.000000000000000000 ) ) ;
#6976 = DIRECTION ( 'NONE',  ( 1.000000000000000000, 0.000000000000000000, 0.000000000000000000 ) ) ;
#6977 = CARTESIAN_POINT ( 'NONE',  ( -15.40903463028480580, 44.25937500034140015, 47.42413220539094709 ) ) ;
#6978 = LINE ( 'NONE', #5648, #12034 ) ;
#6979 = DIRECTION ( 'NONE',  ( -0.000000000000000000, -1.000000000000000000, -0.000000000000000000 ) ) ;
#6980 = LINE ( 'NONE', #637, #11272 ) ;
#6981 = CARTESIAN_POINT ( 'NONE',  ( -1.240322475938754499E-13, 36.28125000068280315, 50.00000000000000000 ) ) ;
#6982 = CIRCLE ( 'NONE', #8302, 17.50000000000000000 ) ;
#6983 = CARTESIAN_POINT ( 'NONE',  ( 40.45084971874737079, 22.98125000068279888, -29.38926261462366440 ) ) ;
#6984 = CARTESIAN_POINT ( 'NONE',  ( 0.000000000000000000, 50.00000000000000000, 0.000000000000000000 ) ) ;
#6985 = ORIENTED_EDGE ( 'NONE', *, *, #15743, .T. ) ;
#6986 = CARTESIAN_POINT ( 'NONE',  ( 30.81806926056964002, 28.55937500034139731, 42.41743335407647209 ) ) ;
#6987 = ADVANCED_FACE ( 'NONE', ( #15045 ), #5265, .F. ) ;
#6988 = ORIENTED_EDGE ( 'NONE', *, *, #11109, .F. ) ;
#6989 = EDGE_LOOP ( 'NONE', ( #13972, #467, #14488, #7179 ) ) ;
#6990 = ORIENTED_EDGE ( 'NONE', *, *, #10730, .F. ) ;
#6991 = CARTESIAN_POINT ( 'NONE',  ( 30.90169943749475578, 42.48125000068279888, 42.53254041760200010 ) ) ;
#6992 = FACE_BOUND ( 'NONE', #6937, .T. ) ;
#6993 = CARTESIAN_POINT ( 'NONE',  ( 30.81806926056964002, 24.55937500034139376, 42.41743335407647209 ) ) ;
#6995 = ORIENTED_EDGE ( 'NONE', *, *, #6538, .T. ) ;
#6994 = AXIS2_PLACEMENT_3D ( 'NONE', #9160, #9330, #419 ) ;
#6996 = CARTESIAN_POINT ( 'NONE',  ( -7.919222016226816763, 27.33250428222964246, -49.99999999999999289 ) ) ;
#6997 = CARTESIAN_POINT ( 'NONE',  ( -49.99999999999999289, 47.89999999999999858, -16.24598481164531449 ) ) ;
#6998 = DIRECTION ( 'NONE',  ( -0.9361168066628589024, -0.08189960831908940642, -0.3420201433256691015 ) ) ;
#6999 = CARTESIAN_POINT ( 'NONE',  ( 6.123233995736766085E-15, 20.00000000000000355, -50.00000000000000000 ) ) ;
#7000 = CARTESIAN_POINT ( 'NONE',  ( 30.81806926056964002, 30.62187500034139376, 42.41743335407646498 ) ) ;
#7001 = CARTESIAN_POINT ( 'NONE',  ( -7.919222016226804328, 48.44874571845315359, 50.00000000000000000 ) ) ;
#7002 = CARTESIAN_POINT ( 'NONE',  ( -24.78626291527393377, 40.00000000000000711, -5.650101528493794767 ) ) ;
#7003 = CARTESIAN_POINT ( 'NONE',  ( -45.33038492356476468, 20.00000000000001776, 20.77601661419166845 ) ) ;
#7004 = CARTESIAN_POINT ( 'NONE',  ( -49.86468353124999453, 24.02187500034139589, 16.20201782572377169 ) ) ;
#7005 =( BOUNDED_CURVE ( )  B_SPLINE_CURVE ( 2, ( #9046, #5155, #10212, #15264, #8965, #14022, #1132, #11219, #4911, #2638, #7713, #3655, #12782 ),
 .UNSPECIFIED., .F., .F. ) 
 B_SPLINE_CURVE_WITH_KNOTS ( ( 3, 2, 2, 2, 2, 2, 3 ),
 ( 0.4500000000000000111, 0.4533333333333333104, 0.4600000000000000200, 0.4666666666666666741, 0.4733333333333333282, 0.4799999999999999822, 0.4833333333333333370 ),
 .UNSPECIFIED. ) 
 CURVE ( )  GEOMETRIC_REPRESENTATION_ITEM ( )  RATIONAL_B_SPLINE_CURVE ( ( 0.9755282581475768211, 0.9755282581475770431, 1.000000000000000000, 0.9510565162951535312, 1.000000000000000000, 0.9510565162951535312, 1.000000000000000000, 0.9510565162951535312, 1.000000000000000000, 0.9510565162951535312, 1.000000000000000000, 0.9755282581475768211, 0.9755282581475768211 ) ) 
 REPRESENTATION_ITEM ( '' )  );
#7006 = CARTESIAN_POINT ( 'NONE',  ( 4.127528389677815213, 5.486372832567310454, 101.0000000000000000 ) ) ;
#7007 = CARTESIAN_POINT ( 'NONE',  ( 30.90169943749475578, 34.70000000000000995, 42.53254041760200010 ) ) ;
#7008 = CARTESIAN_POINT ( 'NONE',  ( -40.34137639590981905, 23.65937500034139518, -29.30972558990011478 ) ) ;
#7009 = AXIS2_PLACEMENT_3D ( 'NONE', #3245, #4671, #12227 ) ;
#7010 = LINE ( 'NONE', #4597, #10703 ) ;
#7011 = VERTEX_POINT ( 'NONE', #3749 ) ;
#7012 = CARTESIAN_POINT ( 'NONE',  ( 40.34137639590981195, 29.05937500034139376, -29.30972558990011834 ) ) ;
#7013 = ORIENTED_EDGE ( 'NONE', *, *, #8927, .F. ) ;
#7014 = EDGE_CURVE ( 'NONE', #15272, #4817, #4137, .T. ) ;
#7015 = DIRECTION ( 'NONE',  ( -0.000000000000000000, 0.000000000000000000, -1.000000000000000000 ) ) ;
#7016 = CARTESIAN_POINT ( 'NONE',  ( 15.40903463028481113, 43.25937500034139305, -47.42413220539094709 ) ) ;
#7017 = CARTESIAN_POINT ( 'NONE',  ( 50.00000000000000711, 34.89999999999999858, 16.24598481164530739 ) ) ;
#7018 = VECTOR ( 'NONE', #1733, 1000.000000000000114 ) ;
#7019 = CYLINDRICAL_SURFACE ( 'NONE', #12913, 50.00000000000000000 ) ;
#7020 = CARTESIAN_POINT ( 'NONE',  ( 49.86468353124999453, 27.02187500034139589, -16.20201782572376459 ) ) ;
#7021 = CARTESIAN_POINT ( 'NONE',  ( 40.34137639590981905, 34.65937500034139873, 29.30972558990010768 ) ) ;
#7022 = CARTESIAN_POINT ( 'NONE',  ( -3.111920190527341144E-15, 43.50000000000000711, -50.00000000000000000 ) ) ;
#7023 = CARTESIAN_POINT ( 'NONE',  ( -30.81806926056962226, 28.22187500034139873, 42.41743335407647919 ) ) ;
#7024 = DIRECTION ( 'NONE',  ( 0.000000000000000000, 0.000000000000000000, 1.000000000000000000 ) ) ;
#7025 = CARTESIAN_POINT ( 'NONE',  ( -3.210462471511496205E-15, 43.35937500034138736, -52.43083105670540789 ) ) ;
#7026 = CARTESIAN_POINT ( 'NONE',  ( 30.81806926056964002, 46.62187500034140442, 42.41743335407647209 ) ) ;
#7027 = ADVANCED_FACE ( 'NONE', ( #11644 ), #10474, .F. ) ;
#7028 = CARTESIAN_POINT ( 'NONE',  ( -40.34137639590981905, 23.72187500034139873, -29.30972558990011478 ) ) ;
#7029 = ORIENTED_EDGE ( 'NONE', *, *, #6422, .T. ) ;
#7030 = AXIS2_PLACEMENT_3D ( 'NONE', #11309, #10063, #6158 ) ;
#7031 = EDGE_CURVE ( 'NONE', #7298, #15854, #482, .T. ) ;
#7032 = CARTESIAN_POINT ( 'NONE',  ( 15.40903463028481113, 49.25937500034139305, -47.42413220539094709 ) ) ;
#7033 = ORIENTED_EDGE ( 'NONE', *, *, #2049, .F. ) ;
#7034 = EDGE_LOOP ( 'NONE', ( #7555, #13599, #9705, #15205 ) ) ;
#7035 = CARTESIAN_POINT ( 'NONE',  ( -49.99999999999999289, 27.68125000068279462, -16.24598481164531449 ) ) ;
#7036 = ORIENTED_EDGE ( 'NONE', *, *, #9462, .F. ) ;
#7037 = ADVANCED_FACE ( 'NONE', ( #6751 ), #12883, .F. ) ;
#7038 = LINE ( 'NONE', #11769, #13170 ) ;
#7039 = CARTESIAN_POINT ( 'NONE',  ( -40.34137639590981195, 40.12187500034139731, 29.30972558990012189 ) ) ;
#7040 = CARTESIAN_POINT ( 'NONE',  ( 15.40903463028482356, 46.52187500034139589, 47.42413220539093999 ) ) ;
#7041 = CIRCLE ( 'NONE', #4936, 45.00000000000000000 ) ;
#7042 = CARTESIAN_POINT ( 'NONE',  ( -50.00000000000000000, 38.00000000000000711, 0.000000000000000000 ) ) ;
#7043 = CARTESIAN_POINT ( 'NONE',  ( -15.40903463028480580, 38.32187500034140015, 47.42413220539094709 ) ) ;
#7044 = CARTESIAN_POINT ( 'NONE',  ( 17.28626291527370284, 40.00000000000000711, -18.64048258526063151 ) ) ;
#7045 = EDGE_LOOP ( 'NONE', ( #6320, #6988, #6600, #14208 ) ) ;
#7046 = CARTESIAN_POINT ( 'NONE',  ( -30.81806926056963292, 39.62187500034138310, -42.41743335407647209 ) ) ;
#7047 = VERTEX_POINT ( 'NONE', #2826 ) ;
#7048 = ORIENTED_EDGE ( 'NONE', *, *, #14177, .F. ) ;
#7049 = AXIS2_PLACEMENT_3D ( 'NONE', #473, #1567, #9226 ) ;
#7050 = ORIENTED_EDGE ( 'NONE', *, *, #15947, .T. ) ;
#7051 = EDGE_CURVE ( 'NONE', #14108, #13278, #4798, .T. ) ;
#7052 = CARTESIAN_POINT ( 'NONE',  ( 1.034004556265705202E-14, 102.0000000000000142, 9.080892972013893782 ) ) ;
#7053 = DIRECTION ( 'NONE',  ( 1.000000000000000000, -0.000000000000000000, 0.000000000000000000 ) ) ;
#7054 = CARTESIAN_POINT ( 'NONE',  ( -6.725310538855818976, 29.22831317314782851, 101.0000000000000000 ) ) ;
#7055 = CARTESIAN_POINT ( 'NONE',  ( 50.00000000000000000, 36.78125000068280315, -6.123233995736766085E-15 ) ) ;
#7056 = CARTESIAN_POINT ( 'NONE',  ( 15.40903463028481113, 37.25937500034140015, -47.42413220539094709 ) ) ;
#7057 = CARTESIAN_POINT ( 'NONE',  ( -49.86468353124999453, 49.75937500034137884, -16.20201782572375393 ) ) ;
#7058 = EDGE_CURVE ( 'NONE', #2476, #871, #619, .T. ) ;
#7059 = CARTESIAN_POINT ( 'NONE',  ( -40.45084971874737789, 45.79999999999999716, -29.38926261462365730 ) ) ;
#7060 = AXIS2_PLACEMENT_3D ( 'NONE', #944, #10857, #12261 ) ;
#7061 = LINE ( 'NONE', #731, #3563 ) ;
#7062 = LINE ( 'NONE', #5899, #1515 ) ;
#7063 = VECTOR ( 'NONE', #14789, 1000.000000000000000 ) ;
#7064 = CARTESIAN_POINT ( 'NONE',  ( -40.45084971874737079, 34.20000000000000284, 29.38926261462367151 ) ) ;
#7065 = CARTESIAN_POINT ( 'NONE',  ( -7.164845293664018122, 37.36320934111677161, 102.0000000000000142 ) ) ;
#7066 = MECHANICAL_DESIGN_GEOMETRIC_PRESENTATION_REPRESENTATION (  '', ( #3346 ), #5233 ) ;
#7067 = ORIENTED_EDGE ( 'NONE', *, *, #1371, .F. ) ;
#7068 = CARTESIAN_POINT ( 'NONE',  ( 9.631387414534489405E-15, 28.35937500034139802, 52.43083105670540789 ) ) ;
#7069 = VERTEX_POINT ( 'NONE', #5651 ) ;
#7070 = ORIENTED_EDGE ( 'NONE', *, *, #10581, .T. ) ;
#7071 = ORIENTED_EDGE ( 'NONE', *, *, #3249, .F. ) ;
#7072 = CARTESIAN_POINT ( 'NONE',  ( 15.45084971874736723, 45.18125000068280173, -47.55282581475768211 ) ) ;
#7073 = CIRCLE ( 'NONE', #11325, 60.00000000000000711 ) ;
#7074 = AXIS2_PLACEMENT_3D ( 'NONE', #9593, #14640, #9764 ) ;
#7075 = AXIS2_PLACEMENT_3D ( 'NONE', #15062, #9668, #14808 ) ;
#7076 = CARTESIAN_POINT ( 'NONE',  ( -7.164845293664018122, 37.36320934111677161, 102.0000000000000142 ) ) ;
#7077 = LINE ( 'NONE', #14615, #6249 ) ;
#7078 = CIRCLE ( 'NONE', #12108, 17.50000000000000000 ) ;
#7079 = VERTEX_POINT ( 'NONE', #10568 ) ;
#7080 = CARTESIAN_POINT ( 'NONE',  ( 4.898587196589413026E-15, 262.0000000000000000, 40.00000000000000000 ) ) ;
#7081 = CARTESIAN_POINT ( 'NONE',  ( 30.27664397204019409, 40.00000000000000711, -26.14048258526078072 ) ) ;
#7082 = CARTESIAN_POINT ( 'NONE',  ( -30.90169943749473447, 48.30000000000000426, 42.53254041760200721 ) ) ;
#7083 = LINE ( 'NONE', #7327, #11315 ) ;
#7084 = DIRECTION ( 'NONE',  ( 0.000000000000000000, -1.000000000000000000, 0.000000000000000000 ) ) ;
#7085 = DIRECTION ( 'NONE',  ( -0.08715574274765824914, 0.9961946980917455452, 0.000000000000000000 ) ) ;
#7086 = ADVANCED_FACE ( 'NONE', ( #14118 ), #11961, .F. ) ;
#7087 = CARTESIAN_POINT ( 'NONE',  ( 7.857766451448484831E-15, 52.00000000000000711, -63.16733765196516970 ) ) ;
#7088 = EDGE_CURVE ( 'NONE', #12113, #562, #6587, .T. ) ;
#7089 = CARTESIAN_POINT ( 'NONE',  ( 9.735664389687646693E-15, 262.0000000000000000, -79.49773270518484480 ) ) ;
#7090 = CARTESIAN_POINT ( 'NONE',  ( -45.74278786629260907, 19.99999999999998934, 19.85154960931437174 ) ) ;
#7091 = CARTESIAN_POINT ( 'NONE',  ( 30.81806926056962936, 21.22187500034139518, -42.41743335407646498 ) ) ;
#7092 = CARTESIAN_POINT ( 'NONE',  ( 0.5000000000000009992, 31.99999999999998579, 102.0000000000000142 ) ) ;
#7093 = AXIS2_PLACEMENT_3D ( 'NONE', #7590, #12669, #15315 ) ;
#7094 = CARTESIAN_POINT ( 'NONE',  ( 30.90169943749474157, 27.29999999999999716, -42.53254041760200721 ) ) ;
#7095 = CARTESIAN_POINT ( 'NONE',  ( 49.86468353124999453, 22.95937500034139589, -16.20201782572376459 ) ) ;
#7096 = CIRCLE ( 'NONE', #10271, 16.50000000000000711 ) ;
#7097 = CIRCLE ( 'NONE', #3108, 2.000000000000001776 ) ;
#7098 = CARTESIAN_POINT ( 'NONE',  ( 7.580410092413998768, 99.32916037694960210, -5.000000000000000000 ) ) ;
#7099 = ORIENTED_EDGE ( 'NONE', *, *, #11253, .F. ) ;
#7100 = UNCERTAINTY_MEASURE_WITH_UNIT (LENGTH_MEASURE( 1.000000000000000082E-05 ), #976, 'distance_accuracy_value', 'NONE');
#7101 = CARTESIAN_POINT ( 'NONE',  ( -30.81806926056962226, 26.15937500034139163, 42.41743335407647209 ) ) ;
#7102 = ORIENTED_EDGE ( 'NONE', *, *, #12301, .T. ) ;
#7103 = CYLINDRICAL_SURFACE ( 'NONE', #14769, 50.00000000000000000 ) ;
#7104 = CARTESIAN_POINT ( 'NONE',  ( -15.40903463028480580, 36.25937500034140015, 47.42413220539094709 ) ) ;
#7105 = AXIS2_PLACEMENT_3D ( 'NONE', #3311, #11050, #14858 ) ;
#7106 = CARTESIAN_POINT ( 'NONE',  ( -7.580410092413979228, 99.32916037694960210, -5.000000000000000000 ) ) ;
#7107 = CARTESIAN_POINT ( 'NONE',  ( 15.45084971874737789, 34.60000000000000853, 47.55282581475767500 ) ) ;
#7108 =( BOUNDED_SURFACE ( )  B_SPLINE_SURFACE ( 1, 2, ( 
 ( #5140, #4036, #5308, #1195, #11363, #6459, #7857, #12690, #5222, #16430, #10356, #5064, #12936, #8948, #14004, #1541, #10440, #15496, #10116, #15166, #3795, #8858, #13917, #2536, #7616, #7940, #527, #15913, #13255, #11843, #6951, #1617, #6794, #7026, #4369, #8190, #15827, #4212, #2950, #602, #8098, #4458, #6709, #12081, #4537, #14253, #5550, #13014, #1855, #9434, #2873, #11761, #13331, #1935, #3117, #12006, #5462, #14333, #6876, #9354, #5624, #360, #10528, #15669, #15587, #688, #10849, #9279, #8017, #13092, #1697, #5696, #4291, #14485, #449, #10764, #10612, #14405, #3027, #9523, #13176, #11927, #1783, #3194, #10685, #15740, #14570, #8267, #5782, #2103, #6033, #9851, #12506, #7364, #6191, #855, #12428, #11186, #7191, #7440, #12333, #934, #16241, #2022, #13495, #11010, #5949, #14647, #9600, #13657, #11106, #11266, #12173, #4875, #12252, #9932, #7277, #14985, #5863, #16165, #8511, #4709, #16073, #9771, #7116, #10927, #16323, #4795, #1021, #3276, #14903, #14818, #2180, #3449, #13576, #2357, #3530, #1098, #3614, #8583, #6116, #8345, #14729, #13406, #2266, #8678, #13744, #773, #15990, #4616, #3361, #9679, #8432, #11425, #5199, #13986, #13821, #6612, #2763, #2683, #5122, #2433, #14067, #6520, #15073, #7757, #15318, #7510, #10256, #3938, #8921, #9011, #1269, #3776, #7680, #185, #10340, #2514, #8835, #12750, #10175, #7594, #1347, #15402, #12827, #4021, #18, #12582, #1430, #13899, #11667, #6438, #11499, #96, #5289, #9090, #12672, #2604, #3702, #14147, #8759, #11580, #7839, #12914, #3855, #15225, #1523, #4959, #10019, #1179, #6275, #11347, #16413, #5046, #10099, #15150, #6361, #9171, #15478, #12997, #2854, #5368, #7921, #10424, #263, #4100, #14230, #1600, #6694, #8521, #16093, #14998, #14833, #12519, #16004, #13589, #2369, #2115, #16252, #3289, #866, #12348, #3461, #9613, #16180, #14661, #2194, #7203, #12265, #4810, #11119, #9861, #8359, #1110, #2038, #15928, #14914, #3543, #13428, #7128, #7291, #6206, #8597, #13508, #13672, #12186, #8446, #8690, #6047, #2284, #1032, #5877, #4630, #7376, #9787, #6130, #786, #13756, #4549, #10939, #5961, #9694, #12440, #11200, #14746, #3379, #3633, #7452, #4887, #9943, #11024, #4726, #949, #6375, #2621, #16336, #12933, #12688, #1538, #9104, #7855 ),
 ( #11277, #7614, #15087, #1448, #4975, #8944, #11361, #200, #5138, #10034, #10114, #3791, #2448, #8856, #7696, #11515, #14164, #9027, #3714, #2533, #14081, #12845, #13915, #2780, #14002, #12766, #6537, #8772, #15164, #1285, #11440, #13834, #7526, #15334, #1365, #12598, #1193, #11602, #3953, #10354, #6292, #15416, #33, #16427, #5062, #5305, #10193, #7773, #15246, #6456, #4034, #3872, #111, #5219, #2697, #10279, #5382, #447, #3115, #358, #9432, #8265, #8096, #14331, #15666, #2948, #6792, #15825, #3025, #4456, #8187, #8015, #14483, #10437, #11757, #9521, #4210, #13089, #1695, #6949, #13253, #10762, #5459, #5548, #15493, #11838, #6874, #4289, #4118, #13329, #14568, #4367, #10610, #9189, #15736, #1853, #278, #12003, #525, #14251, #11925, #5620, #9352, #10683, #14402, #10526, #13174, #599, #5694, #9276, #15585, #1780, #3192, #6629, #11680, #2870, #7938, #13012, #1614, #6707, #10592, #6933, #6692, #5762, #11985, #5676, #9258, #1677, #10669, #13152, #9416, #11740, #3254, #3009, #8324, #15895, #14629, #10505, #6777, #11820, #1598, #582, #8080, #1837, #5531, #10746, #343, #14388, #5442, #8248, #15564, #15720, #427, #7007, #11909, #4194, #15648, #4272, #14314, #9338, #14461, #15804, #4519, #4434, #2933, #1760, #9505, #3177, #6862, #9584, #4351, #3095, #13313, #8000, #509, #5604, #8171, #13074, #13239, #14550, #1912, #12063, #665, #10831, #997, #12486, #3678, #5845, #9657, #15049, #16145, #16221, #13389, #14881, #4682, #6009, #9751, #13556, #6170, #9832, #11243, #14964, #14796, #4853, #12153, #2084, #16299, #10987, #3430, #8491, #13719, #3591, #1078, #7173, #12311, #754, #2162, #13634, #11077, #10908, #1997, #4937, #11166, #7254, #15972, #6098, #8649, #7094, #9910, #7336, #4593, #2246, #12406, #912, #2336, #4773, #12234, #3511, #7417, #9991, #16052, #837, #8564, #14707, #3338, #8410, #13478, #5928, #14123, #5268, #1405, #1244, #14045, #13800, #12887, #2662, #12802, #16388, #8813, #1324, #3833, #72, #2412, #10400, #10151, #15457, #6591, #5347, #1156, #13877, #2493, #8734, #7736, #15203, #8986, #12646, #6496, #7490, #5098, #12560, #15375, #6250, #6414, #7570, #2737, #2582, #11321, #6338, #11402, #5022, #8128, #5177, #11553, #11647, #160, #10074, #8899, #10318, #3998, #13961, #241 ) ),
 .UNSPECIFIED., .F., .F., .F. ) 
 B_SPLINE_SURFACE_WITH_KNOTS ( ( 2, 2 ),
 ( 3, 2, 2, 2, 2, 2, 2, 2, 2, 2, 2, 2, 2, 2, 2, 2, 2, 2, 2, 2, 2, 2, 2, 2, 2, 2, 2, 2, 2, 2, 2, 2, 2, 2, 2, 2, 2, 2, 2, 2, 2, 2, 2, 2, 2, 2, 2, 2, 2, 2, 2, 2, 2, 2, 2, 2, 2, 2, 2, 2, 2, 2, 2, 2, 2, 2, 2, 2, 2, 2, 2, 2, 2, 2, 2, 2, 2, 2, 2, 2, 2, 2, 2, 2, 2, 2, 2, 2, 2, 2, 2, 2, 2, 2, 2, 2, 2, 2, 2, 2, 2, 2, 2, 2, 2, 2, 2, 2, 2, 2, 2, 2, 2, 2, 2, 2, 2, 2, 2, 2, 2, 2, 2, 2, 2, 2, 2, 2, 2, 2, 2, 2, 2, 2, 2, 2, 2, 2, 2, 2, 2, 2, 2, 2, 2, 2, 2, 2, 2, 2, 3 ),
 ( 0.000000000000000000, 1.000000000000000000 ),
 ( 0.000000000000000000, 0.006666666666666667095, 0.01333333333333333419, 0.02000000000000000042, 0.02666666666666666838, 0.03333333333333333287, 0.04000000000000000083, 0.04666666666666666879, 0.05333333333333333676, 0.05999999999999999778, 0.06666666666666666574, 0.07333333333333333370, 0.08000000000000000167, 0.08666666666666666963, 0.09333333333333333759, 0.1000000000000000056, 0.1066666666666666735, 0.1133333333333333276, 0.1199999999999999956, 0.1266666666666666774, 0.1333333333333333315, 0.1400000000000000133, 0.1466666666666666674, 0.1533333333333333215, 0.1600000000000000033, 0.1666666666666666574, 0.1733333333333333393, 0.1799999999999999933, 0.1866666666666666752, 0.1933333333333333293, 0.2000000000000000111, 0.2066666666666666652, 0.2133333333333333470, 0.2200000000000000011, 0.2266666666666666552, 0.2333333333333333370, 0.2399999999999999911, 0.2466666666666666730, 0.2533333333333333548, 0.2600000000000000089, 0.2666666666666666630, 0.2733333333333333171, 0.2800000000000000266, 0.2866666666666666807, 0.2933333333333333348, 0.2999999999999999889, 0.3066666666666666430, 0.3133333333333333526, 0.3200000000000000067, 0.3266666666666666607, 0.3333333333333333148, 0.3400000000000000244, 0.3466666666666666785, 0.3533333333333333326, 0.3599999999999999867, 0.3666666666666666408, 0.3733333333333333504, 0.3800000000000000044, 0.3866666666666666585, 0.3933333333333333126, 0.4000000000000000222, 0.4066666666666666763, 0.4133333333333333304, 0.4199999999999999845, 0.4266666666666666941, 0.4333333333333333481, 0.4400000000000000022, 0.4466666666666666563, 0.4533333333333333104, 0.4600000000000000200, 0.4666666666666666741, 0.4733333333333333282, 0.4799999999999999822, 0.4866666666666666918, 0.4933333333333333459, 0.5000000000000000000, 0.5066666666666667096, 0.5133333333333333082, 0.5200000000000000178, 0.5266666666666666163, 0.5333333333333333259, 0.5400000000000000355, 0.5466666666666666341, 0.5533333333333333437, 0.5600000000000000533, 0.5666666666666666519, 0.5733333333333333615, 0.5799999999999999600, 0.5866666666666666696, 0.5933333333333333792, 0.5999999999999999778, 0.6066666666666666874, 0.6133333333333332860, 0.6199999999999999956, 0.6266666666666667052, 0.6333333333333333037, 0.6400000000000000133, 0.6466666666666666119, 0.6533333333333333215, 0.6600000000000000311, 0.6666666666666666297, 0.6733333333333333393, 0.6800000000000000488, 0.6866666666666666474, 0.6933333333333333570, 0.6999999999999999556, 0.7066666666666666652, 0.7133333333333333748, 0.7199999999999999734, 0.7266666666666666829, 0.7333333333333332815, 0.7399999999999999911, 0.7466666666666667007, 0.7533333333333332993, 0.7600000000000000089, 0.7666666666666667185, 0.7733333333333333171, 0.7800000000000000266, 0.7866666666666666252, 0.7933333333333333348, 0.8000000000000000444, 0.8066666666666666430, 0.8133333333333333526, 0.8199999999999999512, 0.8266666666666666607, 0.8333333333333333703, 0.8399999999999999689, 0.8466666666666666785, 0.8533333333333333881, 0.8599999999999999867, 0.8666666666666666963, 0.8733333333333332948, 0.8800000000000000044, 0.8866666666666667140, 0.8933333333333333126, 0.9000000000000000222, 0.9066666666666666208, 0.9133333333333333304, 0.9200000000000000400, 0.9266666666666666385, 0.9333333333333333481, 0.9399999999999999467, 0.9466666666666666563, 0.9533333333333333659, 0.9599999999999999645, 0.9666666666666666741, 0.9733333333333333837, 0.9799999999999999822, 0.9866666666666666918, 0.9933333333333332904, 1.000000000000000000 ),
 .UNSPECIFIED. ) 
 GEOMETRIC_REPRESENTATION_ITEM ( )  RATIONAL_B_SPLINE_SURFACE ( (
 ( 1.000000000000000000, 0.9510565162951535312, 1.000000000000000000, 0.9510565162951535312, 1.000000000000000000, 0.9510565162951535312, 1.000000000000000000, 0.9510565162951535312, 1.000000000000000000, 0.9510565162951535312, 1.000000000000000000, 0.9510565162951535312, 1.000000000000000000, 0.9510565162951535312, 1.000000000000000000, 0.9510565162951535312, 1.000000000000000000, 0.9510565162951535312, 1.000000000000000000, 0.9510565162951535312, 1.000000000000000000, 0.9510565162951535312, 1.000000000000000000, 0.9510565162951535312, 1.000000000000000000, 0.9510565162951535312, 1.000000000000000000, 0.9510565162951535312, 1.000000000000000000, 0.9510565162951535312, 1.000000000000000000, 0.9510565162951535312, 1.000000000000000000, 0.9510565162951535312, 1.000000000000000000, 0.9510565162951535312, 1.000000000000000000, 0.9510565162951535312, 1.000000000000000000, 0.9510565162951535312, 1.000000000000000000, 0.9510565162951535312, 1.000000000000000000, 0.9510565162951535312, 1.000000000000000000, 0.9510565162951535312, 1.000000000000000000, 0.9510565162951535312, 1.000000000000000000, 0.9510565162951535312, 1.000000000000000000, 0.9510565162951535312, 1.000000000000000000, 0.9510565162951535312, 1.000000000000000000, 0.9510565162951535312, 1.000000000000000000, 0.9510565162951535312, 1.000000000000000000, 0.9510565162951535312, 1.000000000000000000, 0.9510565162951535312, 1.000000000000000000, 0.9510565162951535312, 1.000000000000000000, 0.9510565162951535312, 1.000000000000000000, 0.9510565162951535312, 1.000000000000000000, 0.9510565162951535312, 1.000000000000000000, 0.9510565162951535312, 1.000000000000000000, 0.9510565162951535312, 1.000000000000000000, 0.9510565162951535312, 1.000000000000000000, 0.9510565162951535312, 1.000000000000000000, 0.9510565162951535312, 1.000000000000000000, 0.9510565162951535312, 1.000000000000000000, 0.9510565162951535312, 1.000000000000000000, 0.9510565162951535312, 1.000000000000000000, 0.9510565162951535312, 1.000000000000000000, 0.9510565162951535312, 1.000000000000000000, 0.9510565162951535312, 1.000000000000000000, 0.9510565162951535312, 1.000000000000000000, 0.9510565162951535312, 1.000000000000000000, 0.9510565162951535312, 1.000000000000000000, 0.9510565162951535312, 1.000000000000000000, 0.9510565162951535312, 1.000000000000000000, 0.9510565162951535312, 1.000000000000000000, 0.9510565162951535312, 1.000000000000000000, 0.9510565162951535312, 1.000000000000000000, 0.9510565162951535312, 1.000000000000000000, 0.9510565162951535312, 1.000000000000000000, 0.9510565162951535312, 1.000000000000000000, 0.9510565162951535312, 1.000000000000000000, 0.9510565162951535312, 1.000000000000000000, 0.9510565162951535312, 1.000000000000000000, 0.9510565162951535312, 1.000000000000000000, 0.9510565162951535312, 1.000000000000000000, 0.9510565162951535312, 1.000000000000000000, 0.9510565162951535312, 1.000000000000000000, 0.9510565162951535312, 1.000000000000000000, 0.9510565162951535312, 1.000000000000000000, 0.9510565162951535312, 1.000000000000000000, 0.9510565162951535312, 1.000000000000000000, 0.9510565162951535312, 1.000000000000000000, 0.9510565162951535312, 1.000000000000000000, 0.9510565162951535312, 1.000000000000000000, 0.9510565162951535312, 1.000000000000000000, 0.9510565162951535312, 1.000000000000000000, 0.9510565162951535312, 1.000000000000000000, 0.9510565162951535312, 1.000000000000000000, 0.9510565162951535312, 1.000000000000000000, 0.9510565162951535312, 1.000000000000000000, 0.9510565162951535312, 1.000000000000000000, 0.9510565162951535312, 1.000000000000000000, 0.9510565162951535312, 1.000000000000000000, 0.9510565162951535312, 1.000000000000000000, 0.9510565162951535312, 1.000000000000000000, 0.9510565162951535312, 1.000000000000000000, 0.9510565162951535312, 1.000000000000000000, 0.9510565162951535312, 1.000000000000000000, 0.9510565162951535312, 1.000000000000000000, 0.9510565162951535312, 1.000000000000000000, 0.9510565162951535312, 1.000000000000000000, 0.9510565162951535312, 1.000000000000000000, 0.9510565162951535312, 1.000000000000000000, 0.9510565162951535312, 1.000000000000000000, 0.9510565162951535312, 1.000000000000000000, 0.9510565162951535312, 1.000000000000000000, 0.9510565162951535312, 1.000000000000000000, 0.9510565162951535312, 1.000000000000000000, 0.9510565162951535312, 1.000000000000000000, 0.9510565162951535312, 1.000000000000000000, 0.9510565162951535312, 1.000000000000000000, 0.9510565162951535312, 1.000000000000000000, 0.9510565162951535312, 1.000000000000000000, 0.9510565162951535312, 1.000000000000000000, 0.9510565162951535312, 1.000000000000000000, 0.9510565162951535312, 1.000000000000000000, 0.9510565162951535312, 1.000000000000000000, 0.9510565162951535312, 1.000000000000000000, 0.9510565162951535312, 1.000000000000000000, 0.9510565162951535312, 1.000000000000000000, 0.9510565162951535312, 1.000000000000000000, 0.9510565162951535312, 1.000000000000000000, 0.9510565162951535312, 1.000000000000000000, 0.9510565162951535312, 1.000000000000000000, 0.9510565162951535312, 1.000000000000000000, 0.9510565162951535312, 1.000000000000000000, 0.9510565162951535312, 1.000000000000000000, 0.9510565162951535312, 1.000000000000000000, 0.9510565162951535312, 1.000000000000000000, 0.9510565162951535312, 1.000000000000000000, 0.9510565162951535312, 1.000000000000000000, 0.9510565162951535312, 1.000000000000000000, 0.9510565162951535312, 1.000000000000000000, 0.9510565162951535312, 1.000000000000000000, 0.9510565162951535312, 1.000000000000000000, 0.9510565162951535312, 1.000000000000000000, 0.9510565162951535312, 1.000000000000000000, 0.9510565162951535312, 1.000000000000000000, 0.9510565162951535312, 1.000000000000000000, 0.9510565162951535312, 1.000000000000000000, 0.9510565162951535312, 1.000000000000000000, 0.9510565162951535312, 1.000000000000000000, 0.9510565162951535312, 1.000000000000000000, 0.9510565162951535312, 1.000000000000000000, 0.9510565162951535312, 1.000000000000000000, 0.9510565162951535312, 1.000000000000000000, 0.9510565162951535312, 1.000000000000000000, 0.9510565162951535312, 1.000000000000000000, 0.9510565162951535312, 1.000000000000000000, 0.9510565162951535312, 1.000000000000000000, 0.9510565162951535312, 1.000000000000000000, 0.9510565162951535312, 1.000000000000000000, 0.9510565162951535312, 1.000000000000000000, 0.9510565162951535312, 1.000000000000000000, 0.9510565162951535312, 1.000000000000000000, 0.9510565162951535312, 1.000000000000000000, 0.9510565162951535312, 1.000000000000000000, 0.9510565162951535312, 1.000000000000000000, 0.9510565162951535312, 1.000000000000000000, 0.9510565162951535312, 1.000000000000000000, 0.9510565162951535312, 1.000000000000000000, 0.9510565162951535312, 1.000000000000000000, 0.9510565162951535312, 1.000000000000000000),
 ( 1.000000000000000000, 0.9510565162951535312, 1.000000000000000000, 0.9510565162951535312, 1.000000000000000000, 0.9510565162951535312, 1.000000000000000000, 0.9510565162951535312, 1.000000000000000000, 0.9510565162951535312, 1.000000000000000000, 0.9510565162951535312, 1.000000000000000000, 0.9510565162951535312, 1.000000000000000000, 0.9510565162951535312, 1.000000000000000000, 0.9510565162951535312, 1.000000000000000000, 0.9510565162951535312, 1.000000000000000000, 0.9510565162951535312, 1.000000000000000000, 0.9510565162951535312, 1.000000000000000000, 0.9510565162951535312, 1.000000000000000000, 0.9510565162951535312, 1.000000000000000000, 0.9510565162951535312, 1.000000000000000000, 0.9510565162951535312, 1.000000000000000000, 0.9510565162951535312, 1.000000000000000000, 0.9510565162951535312, 1.000000000000000000, 0.9510565162951535312, 1.000000000000000000, 0.9510565162951535312, 1.000000000000000000, 0.9510565162951535312, 1.000000000000000000, 0.9510565162951535312, 1.000000000000000000, 0.9510565162951535312, 1.000000000000000000, 0.9510565162951535312, 1.000000000000000000, 0.9510565162951535312, 1.000000000000000000, 0.9510565162951535312, 1.000000000000000000, 0.9510565162951535312, 1.000000000000000000, 0.9510565162951535312, 1.000000000000000000, 0.9510565162951535312, 1.000000000000000000, 0.9510565162951535312, 1.000000000000000000, 0.9510565162951535312, 1.000000000000000000, 0.9510565162951535312, 1.000000000000000000, 0.9510565162951535312, 1.000000000000000000, 0.9510565162951535312, 1.000000000000000000, 0.9510565162951535312, 1.000000000000000000, 0.9510565162951535312, 1.000000000000000000, 0.9510565162951535312, 1.000000000000000000, 0.9510565162951535312, 1.000000000000000000, 0.9510565162951535312, 1.000000000000000000, 0.9510565162951535312, 1.000000000000000000, 0.9510565162951535312, 1.000000000000000000, 0.9510565162951535312, 1.000000000000000000, 0.9510565162951535312, 1.000000000000000000, 0.9510565162951535312, 1.000000000000000000, 0.9510565162951535312, 1.000000000000000000, 0.9510565162951535312, 1.000000000000000000, 0.9510565162951535312, 1.000000000000000000, 0.9510565162951535312, 1.000000000000000000, 0.9510565162951535312, 1.000000000000000000, 0.9510565162951535312, 1.000000000000000000, 0.9510565162951535312, 1.000000000000000000, 0.9510565162951535312, 1.000000000000000000, 0.9510565162951535312, 1.000000000000000000, 0.9510565162951535312, 1.000000000000000000, 0.9510565162951535312, 1.000000000000000000, 0.9510565162951535312, 1.000000000000000000, 0.9510565162951535312, 1.000000000000000000, 0.9510565162951535312, 1.000000000000000000, 0.9510565162951535312, 1.000000000000000000, 0.9510565162951535312, 1.000000000000000000, 0.9510565162951535312, 1.000000000000000000, 0.9510565162951535312, 1.000000000000000000, 0.9510565162951535312, 1.000000000000000000, 0.9510565162951535312, 1.000000000000000000, 0.9510565162951535312, 1.000000000000000000, 0.9510565162951535312, 1.000000000000000000, 0.9510565162951535312, 1.000000000000000000, 0.9510565162951535312, 1.000000000000000000, 0.9510565162951535312, 1.000000000000000000, 0.9510565162951535312, 1.000000000000000000, 0.9510565162951535312, 1.000000000000000000, 0.9510565162951535312, 1.000000000000000000, 0.9510565162951535312, 1.000000000000000000, 0.9510565162951535312, 1.000000000000000000, 0.9510565162951535312, 1.000000000000000000, 0.9510565162951535312, 1.000000000000000000, 0.9510565162951535312, 1.000000000000000000, 0.9510565162951535312, 1.000000000000000000, 0.9510565162951535312, 1.000000000000000000, 0.9510565162951535312, 1.000000000000000000, 0.9510565162951535312, 1.000000000000000000, 0.9510565162951535312, 1.000000000000000000, 0.9510565162951535312, 1.000000000000000000, 0.9510565162951535312, 1.000000000000000000, 0.9510565162951535312, 1.000000000000000000, 0.9510565162951535312, 1.000000000000000000, 0.9510565162951535312, 1.000000000000000000, 0.9510565162951535312, 1.000000000000000000, 0.9510565162951535312, 1.000000000000000000, 0.9510565162951535312, 1.000000000000000000, 0.9510565162951535312, 1.000000000000000000, 0.9510565162951535312, 1.000000000000000000, 0.9510565162951535312, 1.000000000000000000, 0.9510565162951535312, 1.000000000000000000, 0.9510565162951535312, 1.000000000000000000, 0.9510565162951535312, 1.000000000000000000, 0.9510565162951535312, 1.000000000000000000, 0.9510565162951535312, 1.000000000000000000, 0.9510565162951535312, 1.000000000000000000, 0.9510565162951535312, 1.000000000000000000, 0.9510565162951535312, 1.000000000000000000, 0.9510565162951535312, 1.000000000000000000, 0.9510565162951535312, 1.000000000000000000, 0.9510565162951535312, 1.000000000000000000, 0.9510565162951535312, 1.000000000000000000, 0.9510565162951535312, 1.000000000000000000, 0.9510565162951535312, 1.000000000000000000, 0.9510565162951535312, 1.000000000000000000, 0.9510565162951535312, 1.000000000000000000, 0.9510565162951535312, 1.000000000000000000, 0.9510565162951535312, 1.000000000000000000, 0.9510565162951535312, 1.000000000000000000, 0.9510565162951535312, 1.000000000000000000, 0.9510565162951535312, 1.000000000000000000, 0.9510565162951535312, 1.000000000000000000, 0.9510565162951535312, 1.000000000000000000, 0.9510565162951535312, 1.000000000000000000, 0.9510565162951535312, 1.000000000000000000, 0.9510565162951535312, 1.000000000000000000, 0.9510565162951535312, 1.000000000000000000, 0.9510565162951535312, 1.000000000000000000, 0.9510565162951535312, 1.000000000000000000, 0.9510565162951535312, 1.000000000000000000, 0.9510565162951535312, 1.000000000000000000, 0.9510565162951535312, 1.000000000000000000, 0.9510565162951535312, 1.000000000000000000, 0.9510565162951535312, 1.000000000000000000, 0.9510565162951535312, 1.000000000000000000, 0.9510565162951535312, 1.000000000000000000, 0.9510565162951535312, 1.000000000000000000, 0.9510565162951535312, 1.000000000000000000, 0.9510565162951535312, 1.000000000000000000, 0.9510565162951535312, 1.000000000000000000, 0.9510565162951535312, 1.000000000000000000, 0.9510565162951535312, 1.000000000000000000, 0.9510565162951535312, 1.000000000000000000, 0.9510565162951535312, 1.000000000000000000, 0.9510565162951535312, 1.000000000000000000, 0.9510565162951535312, 1.000000000000000000, 0.9510565162951535312, 1.000000000000000000, 0.9510565162951535312, 1.000000000000000000, 0.9510565162951535312, 1.000000000000000000, 0.9510565162951535312, 1.000000000000000000, 0.9510565162951535312, 1.000000000000000000, 0.9510565162951535312, 1.000000000000000000, 0.9510565162951535312, 1.000000000000000000, 0.9510565162951535312, 1.000000000000000000, 0.9510565162951535312, 1.000000000000000000, 0.9510565162951535312, 1.000000000000000000, 0.9510565162951535312, 1.000000000000000000) ) ) 
 REPRESENTATION_ITEM ( '' )  SURFACE ( )  );
#7109 = FACE_OUTER_BOUND ( 'NONE', #15075, .T. ) ;
#7110 = CARTESIAN_POINT ( 'NONE',  ( -49.86468353124999453, 31.82187500034139305, -16.20201782572375393 ) ) ;
#7111 = CARTESIAN_POINT ( 'NONE',  ( -40.34137639590981195, 28.05937500034139731, 29.30972558990012189 ) ) ;
#7112 = DIRECTION ( 'NONE',  ( -0.000000000000000000, -0.000000000000000000, -1.000000000000000000 ) ) ;
#7113 = CARTESIAN_POINT ( 'NONE',  ( -40.34137639590981905, 29.72187500034139518, -29.30972558990011478 ) ) ;
#7114 = CARTESIAN_POINT ( 'NONE',  ( 2.600676159226420495E-13, 33.49999999999999289, -49.99999999999999289 ) ) ;
#7115 = CARTESIAN_POINT ( 'NONE',  ( -30.81806926056962226, 46.15937500034139873, 42.41743335407647919 ) ) ;
#7116 = CARTESIAN_POINT ( 'NONE',  ( -15.40903463028481646, 37.52187500034139589, -47.42413220539093999 ) ) ;
#7117 = CARTESIAN_POINT ( 'NONE',  ( 15.40903463028481113, 23.32187500034139660, -47.42413220539094709 ) ) ;
#7118 = ORIENTED_EDGE ( 'NONE', *, *, #2223, .T. ) ;
#7119 = CARTESIAN_POINT ( 'NONE',  ( -3.210462471511496205E-15, 41.35937500034138736, -52.43083105670540789 ) ) ;
#7120 = EDGE_LOOP ( 'NONE', ( #11308, #10341, #2475, #14945, #15875 ) ) ;
#7121 = CARTESIAN_POINT ( 'NONE',  ( 30.90169943749475578, 32.48125000068280599, 42.53254041760200010 ) ) ;
#7122 = ORIENTED_EDGE ( 'NONE', *, *, #9357, .F. ) ;
#7123 = ADVANCED_FACE ( 'NONE', ( #14288, #9313 ), #5582, .T. ) ;
#7124 = DIRECTION ( 'NONE',  ( 0.2079116908177531531, 0.9781476007338069101, 0.000000000000000000 ) ) ;
#7125 = CARTESIAN_POINT ( 'NONE',  ( -49.86468353124999453, 43.82187500034140015, -16.20201782572375393 ) ) ;
#7126 = CARTESIAN_POINT ( 'NONE',  ( 15.40903463028481113, 49.32187500034139305, -47.42413220539094709 ) ) ;
#7127 = CARTESIAN_POINT ( 'NONE',  ( -3.111920190527341144E-15, 25.50000000000000355, -50.00000000000000000 ) ) ;
#7128 = CARTESIAN_POINT ( 'NONE',  ( -49.86468353124999453, 24.02187500034139589, 16.20201782572377525 ) ) ;
#7129 = CARTESIAN_POINT ( 'NONE',  ( 40.45084971874737079, 39.19999999999999574, -29.38926261462366440 ) ) ;
#7130 = ADVANCED_FACE ( 'NONE', ( #11796 ), #15453, .F. ) ;
#7131 = CARTESIAN_POINT ( 'NONE',  ( -49.86468353125000164, 37.92187500034140157, 0.000000000000000000 ) ) ;
#7132 = CARTESIAN_POINT ( 'NONE',  ( 6.123233995736766085E-15, 20.00000000000000355, -50.00000000000000000 ) ) ;
#7133 = ORIENTED_EDGE ( 'NONE', *, *, #15667, .T. ) ;
#7134 = CARTESIAN_POINT ( 'NONE',  ( -3.210462471511496205E-15, 43.42187500034140157, -52.43083105670540789 ) ) ;
#7135 = EDGE_CURVE ( 'NONE', #6385, #4580, #10198, .T. ) ;
#7136 = ORIENTED_EDGE ( 'NONE', *, *, #5371, .F. ) ;
#7137 = ORIENTED_EDGE ( 'NONE', *, *, #3465, .F. ) ;
#7138 = VERTEX_POINT ( 'NONE', #6669 ) ;
#7139 = CYLINDRICAL_SURFACE ( 'NONE', #4450, 50.00000000000000000 ) ;
#7140 = DIRECTION ( 'NONE',  ( 1.000000000000000000, 0.000000000000000000, 0.000000000000000000 ) ) ;
#7141 = EDGE_CURVE ( 'NONE', #2703, #4062, #885, .T. ) ;
#7142 = CARTESIAN_POINT ( 'NONE',  ( 50.00000000000000711, 26.89999999999999858, 16.24598481164530739 ) ) ;
#7143 = DIRECTION ( 'NONE',  ( 1.000000000000000000, -0.000000000000000000, -1.734723475976807094E-17 ) ) ;
#7144 = CARTESIAN_POINT ( 'NONE',  ( 49.86468353124999453, 34.95937500034138878, -16.20201782572376459 ) ) ;
#7145 = CARTESIAN_POINT ( 'NONE',  ( -49.86468353124999453, 45.75937500034140015, -16.20201782572375393 ) ) ;
#7146 = CARTESIAN_POINT ( 'NONE',  ( -2.547328955960238000E-13, 30.49999999999999645, 49.99999999999999289 ) ) ;
#7147 = LINE ( 'NONE', #12459, #2834 ) ;
#7148 = AXIS2_PLACEMENT_3D ( 'NONE', #15694, #9311, #1730 ) ;
#7149 = CARTESIAN_POINT ( 'NONE',  ( -9.500222237632405253, 22.00424054664139817, 102.0000000000000142 ) ) ;
#7150 =( BOUNDED_CURVE ( )  B_SPLINE_CURVE ( 3, ( #14957, #2486, #12796, #8727 ),
 .UNSPECIFIED., .F., .F. ) 
 B_SPLINE_CURVE_WITH_KNOTS ( ( 4, 4 ),
 ( 2.558501865821649623, 3.141592653589793116 ),
 .UNSPECIFIED. ) 
 CURVE ( )  GEOMETRIC_REPRESENTATION_ITEM ( )  RATIONAL_B_SPLINE_CURVE ( ( 1.000000000000000000, 0.9718672150731670900, 0.9718672150731670900, 1.000000000000000000 ) ) 
 REPRESENTATION_ITEM ( '' )  );
#7151 = CARTESIAN_POINT ( 'NONE',  ( -50.00000000000000000, 46.00000000000000000, 0.000000000000000000 ) ) ;
#7152 = CARTESIAN_POINT ( 'NONE',  ( 15.45084971874736723, 43.18125000068280173, -47.55282581475768211 ) ) ;
#7153 = CARTESIAN_POINT ( 'NONE',  ( 30.90169943749475223, 36.70000000000000284, 42.53254041760199300 ) ) ;
#7154 = EDGE_LOOP ( 'NONE', ( #1667, #9461 ) ) ;
#7155 = CARTESIAN_POINT ( 'NONE',  ( 40.34137639590981905, 28.65937500034139873, 29.30972558990010768 ) ) ;
#7156 = EDGE_LOOP ( 'NONE', ( #1225, #5904 ) ) ;
#7157 = ORIENTED_EDGE ( 'NONE', *, *, #13518, .T. ) ;
#7158 = VERTEX_POINT ( 'NONE', #1652 ) ;
#7159 = CARTESIAN_POINT ( 'NONE',  ( 30.90169943749474157, 43.08125000068280031, -42.53254041760200721 ) ) ;
#7160 = AXIS2_PLACEMENT_3D ( 'NONE', #2711, #5321, #12860 ) ;
#7161 = PLANE ( 'NONE',  #11343 ) ;
#7162 = EDGE_CURVE ( 'NONE', #12621, #13460, #395, .T. ) ;
#7163 = ORIENTED_EDGE ( 'NONE', *, *, #7330, .F. ) ;
#7164 = CARTESIAN_POINT ( 'NONE',  ( -1.240322475938754499E-13, 38.28125000068280315, 50.00000000000000000 ) ) ;
#7165 = CARTESIAN_POINT ( 'NONE',  ( -17.50000000000000000, 22.50000000000000000, 94.42467108177066848 ) ) ;
#7166 = DIRECTION ( 'NONE',  ( -6.938893903907231459E-18, 1.000000000000000000, 5.551115123125782702E-17 ) ) ;
#7167 = CARTESIAN_POINT ( 'NONE',  ( 0.000000000000000000, 193.4213562373095385, 0.000000000000000000 ) ) ;
#7168 = FACE_OUTER_BOUND ( 'NONE', #228, .T. ) ;
#7169 = CARTESIAN_POINT ( 'NONE',  ( 50.00000000000000000, 39.00000000000000000, -6.123233995736766085E-15 ) ) ;
#7170 = CARTESIAN_POINT ( 'NONE',  ( 2.267949192431125027, 22.50000000000000000, 100.0000000000000000 ) ) ;
#7171 = CARTESIAN_POINT ( 'NONE',  ( -40.34137639590981905, 25.72187500034139518, -29.30972558990011478 ) ) ;
#7172 = CARTESIAN_POINT ( 'NONE',  ( -1.240322475938754499E-13, 36.50000000000000711, 50.00000000000000000 ) ) ;
#7173 = CARTESIAN_POINT ( 'NONE',  ( 30.90169943749475578, 28.70000000000000284, 42.53254041760200010 ) ) ;
#7174 = CARTESIAN_POINT ( 'NONE',  ( -30.81806926056962226, 28.15937500034139518, 42.41743335407647919 ) ) ;
#7175 = CARTESIAN_POINT ( 'NONE',  ( -50.00000000000000000, 30.00000000000000355, 0.000000000000000000 ) ) ;
#7176 = EDGE_LOOP ( 'NONE', ( #5510, #3838, #1937, #3536, #7459 ) ) ;
#7177 = CARTESIAN_POINT ( 'NONE',  ( -40.34137639590981905, 25.65937500034139518, -29.30972558990011478 ) ) ;
#7178 = EDGE_CURVE ( 'NONE', #2273, #15190, #2985, .T. ) ;
#7179 = ORIENTED_EDGE ( 'NONE', *, *, #6318, .F. ) ;
#7180 = CARTESIAN_POINT ( 'NONE',  ( 0.000000000000000000, 20.00000000000000355, 0.000000000000000000 ) ) ;
#7181 = CARTESIAN_POINT ( 'NONE',  ( -40.34137639590981195, 34.05937500034139731, 29.30972558990012189 ) ) ;
#7182 = CARTESIAN_POINT ( 'NONE',  ( 2.500000000000000000, 247.0000000000000284, 44.93050188902856945 ) ) ;
#7183 = PLANE ( 'NONE',  #15199 ) ;
#7184 = DIRECTION ( 'NONE',  ( 0.000000000000000000, 1.000000000000000000, 0.000000000000000000 ) ) ;
#7185 = CARTESIAN_POINT ( 'NONE',  ( -30.81806926056962226, 32.22187500034139163, 42.41743335407647919 ) ) ;
#7186 = CARTESIAN_POINT ( 'NONE',  ( -30.81806926056962226, 28.15937500034139518, 42.41743335407647209 ) ) ;
#7187 = FACE_OUTER_BOUND ( 'NONE', #10022, .T. ) ;
#7188 = CARTESIAN_POINT ( 'NONE',  ( -15.40903463028481646, 27.52187500034139944, -47.42413220539093999 ) ) ;
#7189 = DIRECTION ( 'NONE',  ( -0.000000000000000000, -0.000000000000000000, -1.000000000000000000 ) ) ;
#7190 = CARTESIAN_POINT ( 'NONE',  ( -49.86468353125000164, 47.85937500034139447, 0.000000000000000000 ) ) ;
#7191 = CARTESIAN_POINT ( 'NONE',  ( -40.34137639590981195, 40.12187500034139731, 29.30972558990012189 ) ) ;
#7192 = CARTESIAN_POINT ( 'NONE',  ( 30.81806926056962936, 23.22187500034139163, -42.41743335407647209 ) ) ;
#7193 = ORIENTED_EDGE ( 'NONE', *, *, #10477, .T. ) ;
#7194 = CARTESIAN_POINT ( 'NONE',  ( 30.81806926056964002, 40.55937500034139731, 42.41743335407646498 ) ) ;
#7195 = ORIENTED_EDGE ( 'NONE', *, *, #9559, .F. ) ;
#7196 = CARTESIAN_POINT ( 'NONE',  ( -40.45084971874737789, 25.58125000068279675, -29.38926261462365730 ) ) ;
#7197 = VERTEX_POINT ( 'NONE', #5815 ) ;
#7198 = PLANE ( 'NONE',  #15820 ) ;
#7199 = CARTESIAN_POINT ( 'NONE',  ( -49.86468353124999453, 39.82187500034140015, -16.20201782572375393 ) ) ;
#7200 = CARTESIAN_POINT ( 'NONE',  ( 15.40903463028481113, 21.25937500034139660, -47.42413220539094709 ) ) ;
#7201 = CARTESIAN_POINT ( 'NONE',  ( 0.000000000000000000, 20.00000000000000355, 0.000000000000000000 ) ) ;
#7202 = EDGE_CURVE ( 'NONE', #7285, #2610, #12591, .T. ) ;
#7203 = CARTESIAN_POINT ( 'NONE',  ( 30.81806926056962936, 25.22187500034139873, -42.41743335407647209 ) ) ;
#7204 = ADVANCED_FACE ( 'NONE', ( #10882 ), #16119, .F. ) ;
#7205 = CARTESIAN_POINT ( 'NONE',  ( 30.90169943749474157, 33.08125000068279320, -42.53254041760200721 ) ) ;
#7206 = CARTESIAN_POINT ( 'NONE',  ( -3.210462471511496205E-15, 41.42187500034140157, -52.43083105670540789 ) ) ;
#7207 = CARTESIAN_POINT ( 'NONE',  ( -30.00000000000000711, 282.0000000000000000, -12.49999999999999822 ) ) ;
#7208 = ORIENTED_EDGE ( 'NONE', *, *, #10278, .T. ) ;
#7209 = CARTESIAN_POINT ( 'NONE',  ( 15.40903463028482356, 42.52187500034139589, 47.42413220539093999 ) ) ;
#7210 = CARTESIAN_POINT ( 'NONE',  ( -40.45084971874737789, 43.58125000068280031, -29.38926261462365730 ) ) ;
#7211 = VERTEX_POINT ( 'NONE', #8467 ) ;
#7212 = ORIENTED_EDGE ( 'NONE', *, *, #6936, .F. ) ;
#7213 = ORIENTED_EDGE ( 'NONE', *, *, #13545, .F. ) ;
#7214 = EDGE_CURVE ( 'NONE', #13541, #3156, #12314, .T. ) ;
#7215 = PRODUCT_DEFINITION ( 'UNKNOWN', '', #3883, #3942 ) ;
#7216 = CARTESIAN_POINT ( 'NONE',  ( -14.90544456622763470, 13.31698729810771376, 101.0000000000000000 ) ) ;
#7217 = CARTESIAN_POINT ( 'NONE',  ( -25.00000000000000355, 312.0000000000000568, 7.500000000000001776 ) ) ;
#7218 = CARTESIAN_POINT ( 'NONE',  ( 40.45084971874737789, 26.80000000000000071, 29.38926261462365375 ) ) ;
#7219 = FACE_OUTER_BOUND ( 'NONE', #611, .T. ) ;
#7220 = CARTESIAN_POINT ( 'NONE',  ( 40.34137639590981905, 36.65937500034139873, 29.30972558990010768 ) ) ;
#7221 = FACE_OUTER_BOUND ( 'NONE', #4556, .T. ) ;
#7222 = CARTESIAN_POINT ( 'NONE',  ( -2.547328955960238000E-13, 24.49999999999999289, 49.99999999999999289 ) ) ;
#7223 = CARTESIAN_POINT ( 'NONE',  ( -7.580410092413954359, 101.3368000520362813, 5.000000000000000000 ) ) ;
#7224 = FILL_AREA_STYLE_COLOUR ( '', #12379 ) ;
#7225 = DIRECTION ( 'NONE',  ( -6.938893903907231459E-18, 1.000000000000000000, 5.551115123125782702E-17 ) ) ;
#7226 = CARTESIAN_POINT ( 'NONE',  ( 1.010305842943185372E-14, 272.0000000000000000, 82.49773270518484480 ) ) ;
#7227 = CARTESIAN_POINT ( 'NONE',  ( 30.90169943749475223, 36.70000000000000284, 42.53254041760199300 ) ) ;
#7228 = FILL_AREA_STYLE_COLOUR ( '', #4056 ) ;
#7229 = ORIENTED_EDGE ( 'NONE', *, *, #13125, .T. ) ;
#7230 = ADVANCED_FACE ( 'NONE', ( #10718 ), #8299, .F. ) ;
#7231 = CARTESIAN_POINT ( 'NONE',  ( 40.34137639590981905, 32.65937500034139873, 29.30972558990010768 ) ) ;
#7232 = CARTESIAN_POINT ( 'NONE',  ( -15.45084971874736368, 48.18125000068280173, 47.55282581475768211 ) ) ;
#7233 = ORIENTED_EDGE ( 'NONE', *, *, #9316, .F. ) ;
#7234 = VERTEX_POINT ( 'NONE', #4404 ) ;
#7235 = CARTESIAN_POINT ( 'NONE',  ( -30.90169943749473802, 42.08125000068279320, 42.53254041760200721 ) ) ;
#7236 = CARTESIAN_POINT ( 'NONE',  ( -9.881733417930727015, 8.048309972292139847, 102.0000000000000142 ) ) ;
#7237 = DIRECTION ( 'NONE',  ( 0.000000000000000000, -0.000000000000000000, -1.000000000000000000 ) ) ;
#7238 = VERTEX_POINT ( 'NONE', #887 ) ;
#7239 = CARTESIAN_POINT ( 'NONE',  ( 7.919222016226875382, 39.22999571913595673, -49.99999999999997158 ) ) ;
#7240 = ADVANCED_FACE ( 'NONE', ( #13534, #2137 ), #14683, .T. ) ;
#7241 = DIRECTION ( 'NONE',  ( 0.000000000000000000, 0.000000000000000000, 1.000000000000000000 ) ) ;
#7242 = CARTESIAN_POINT ( 'NONE',  ( -17.27575688642330221, 19.64968859734266715, 94.97692319343484257 ) ) ;
#7243 = DIRECTION ( 'NONE',  ( -0.5877852522924689183, -0.8090169943749505599, 0.000000000000000000 ) ) ;
#7244 = LINE ( 'NONE', #8317, #8862 ) ;
#7245 = CYLINDRICAL_SURFACE ( 'NONE', #3163, 50.00000000000000000 ) ;
#7246 =( BOUNDED_CURVE ( )  B_SPLINE_CURVE ( 2, ( #13733, #1589, #15214, #5187, #3843, #14135, #4088, #252, #10242, #2750, #12660, #8909, #10411 ),
 .UNSPECIFIED., .F., .F. ) 
 B_SPLINE_CURVE_WITH_KNOTS ( ( 3, 2, 2, 2, 2, 2, 3 ),
 ( 0.7500000000000000000, 0.7533333333333332993, 0.7600000000000000089, 0.7666666666666667185, 0.7733333333333333171, 0.7800000000000000266, 0.7833333333333333259 ),
 .UNSPECIFIED. ) 
 CURVE ( )  GEOMETRIC_REPRESENTATION_ITEM ( )  RATIONAL_B_SPLINE_CURVE ( ( 0.9755282581475768211, 0.9755282581475768211, 1.000000000000000000, 0.9510565162951535312, 1.000000000000000000, 0.9510565162951535312, 1.000000000000000000, 0.9510565162951535312, 1.000000000000000000, 0.9510565162951535312, 1.000000000000000000, 0.9755282581475768211, 0.9755282581475768211 ) ) 
 REPRESENTATION_ITEM ( '' )  );
#7248 = LINE ( 'NONE', #9578, #7861 ) ;
#7247 = CIRCLE ( 'NONE', #5653, 17.50000000000000000 ) ;
#7249 = EDGE_CURVE ( 'NONE', #14171, #566, #3148, .T. ) ;
#7250 = DIRECTION ( 'NONE',  ( -1.000000000000000000, 0.000000000000000000, 0.000000000000000000 ) ) ;
#7251 = CARTESIAN_POINT ( 'NONE',  ( -40.45084971874737789, 49.58125000068280031, -29.38926261462365730 ) ) ;
#7252 = CARTESIAN_POINT ( 'NONE',  ( 4.898587196589413026E-15, 32.49999999999999289, 40.00000000000000000 ) ) ;
#7253 = B_SPLINE_CURVE_WITH_KNOTS ( 'NONE', 3,
 ( #12418, #1007, #4783, #13644 ),
 .UNSPECIFIED., .F., .F.,
 ( 4, 4 ),
 ( 2.829004760673920638E-07, 0.001414802801989366136 ),
 .UNSPECIFIED. ) ;
#7254 = CARTESIAN_POINT ( 'NONE',  ( -30.90169943749474868, 27.70000000000000284, -42.53254041760200721 ) ) ;
#7255 = CARTESIAN_POINT ( 'NONE',  ( 49.86468353125000164, 26.85937500034139802, -6.106662507704105588E-15 ) ) ;
#7256 = CARTESIAN_POINT ( 'NONE',  ( -15.45084971874737256, 41.38125000068279746, -47.55282581475767500 ) ) ;
#7257 = CARTESIAN_POINT ( 'NONE',  ( 49.86468353124999453, 48.95937500034140299, -16.20201782572376459 ) ) ;
#7258 = ORIENTED_EDGE ( 'NONE', *, *, #12310, .F. ) ;
#7259 = CONICAL_SURFACE ( 'NONE', #9112, 16.50000000000000711, 0.7853981633974447263 ) ;
#7260 = CARTESIAN_POINT ( 'NONE',  ( 9.289494224341416029, 8.863457290943287603, 102.0000000000000142 ) ) ;
#7261 = EDGE_LOOP ( 'NONE', ( #11367, #7208, #545, #4542 ) ) ;
#7262 = CARTESIAN_POINT ( 'NONE',  ( -3.111920190527341144E-15, 43.50000000000000711, -50.00000000000000000 ) ) ;
#7263 = B_SPLINE_CURVE_WITH_KNOTS ( 'NONE', 3,
 ( #5142, #5067, #14256, #2876 ),
 .UNSPECIFIED., .F., .F.,
 ( 4, 4 ),
 ( 2.829004760695596740E-07, 0.001414802801989370690 ),
 .UNSPECIFIED. ) ;
#7264 = CARTESIAN_POINT ( 'NONE',  ( 40.34137639590981905, 34.65937500034139873, 29.30972558990010768 ) ) ;
#7265 = DIRECTION ( 'NONE',  ( 0.000000000000000000, 0.000000000000000000, -1.000000000000000000 ) ) ;
#7266 = EDGE_CURVE ( 'NONE', #605, #7385, #13908, .T. ) ;
#7267 = DIRECTION ( 'NONE',  ( 0.8660254037844362651, 0.000000000000000000, -0.5000000000000041078 ) ) ;
#7268 = CARTESIAN_POINT ( 'NONE',  ( -25.00000000000000711, 286.6727470533916176, 2.499999999998866684 ) ) ;
#7269 = EDGE_CURVE ( 'NONE', #6137, #7369, #8379, .T. ) ;
#7270 = CARTESIAN_POINT ( 'NONE',  ( -40.34137639590981195, 28.12187500034139731, 29.30972558990012189 ) ) ;
#7271 = CARTESIAN_POINT ( 'NONE',  ( 15.40903463028482356, 28.45937500034139589, 47.42413220539093999 ) ) ;
#7272 = CARTESIAN_POINT ( 'NONE',  ( 15.45084971874736723, 27.18125000068279817, -47.55282581475768211 ) ) ;
#7273 = CARTESIAN_POINT ( 'NONE',  ( 30.81806926056962936, 27.22187500034139518, -42.41743335407647209 ) ) ;
#7274 = CARTESIAN_POINT ( 'NONE',  ( -1.671572875253809487, 242.8284271247462129, -50.00000000000000000 ) ) ;
#7275 = VECTOR ( 'NONE', #8643, 1000.000000000000000 ) ;
#7276 = CARTESIAN_POINT ( 'NONE',  ( 15.40903463028481113, 43.25937500034139305, -47.42413220539094709 ) ) ;
#7277 = CARTESIAN_POINT ( 'NONE',  ( -15.40903463028480580, 38.32187500034140015, 47.42413220539094709 ) ) ;
#7278 = CARTESIAN_POINT ( 'NONE',  ( -15.40903463028480580, 22.32187500034139660, 47.42413220539094709 ) ) ;
#7279 = ORIENTED_EDGE ( 'NONE', *, *, #13105, .T. ) ;
#7280 = CARTESIAN_POINT ( 'NONE',  ( 40.34137639590981195, 43.05937500034139731, -29.30972558990011834 ) ) ;
#7281 = ORIENTED_EDGE ( 'NONE', *, *, #15377, .T. ) ;
#7282 = EDGE_CURVE ( 'NONE', #58, #6916, #4492, .T. ) ;
#7283 = CARTESIAN_POINT ( 'NONE',  ( -30.90169943749473802, 22.08125000068279320, 42.53254041760200721 ) ) ;
#7284 = VECTOR ( 'NONE', #7636, 1000.000000000000000 ) ;
#7285 = VERTEX_POINT ( 'NONE', #12284 ) ;
#7286 = EDGE_CURVE ( 'NONE', #894, #12156, #8222, .T. ) ;
#7287 = CARTESIAN_POINT ( 'NONE',  ( -50.00000000000000000, 36.00000000000000711, 0.000000000000000000 ) ) ;
#7288 = CARTESIAN_POINT ( 'NONE',  ( 15.40903463028481113, 33.32187500034139305, -47.42413220539094709 ) ) ;
#7289 = CARTESIAN_POINT ( 'NONE',  ( 40.34137639590981905, 20.65937500034139873, 29.30972558990010768 ) ) ;
#7290 = CARTESIAN_POINT ( 'NONE',  ( -2.939893647802529930, 6.264020653511205516, 102.0000000000000142 ) ) ;
#7291 = CARTESIAN_POINT ( 'NONE',  ( -49.86468353125000164, 23.92187500034139447, 0.000000000000000000 ) ) ;
#7292 = CARTESIAN_POINT ( 'NONE',  ( -15.45084971874736368, 36.18125000068280173, 47.55282581475768211 ) ) ;
#7293 = VECTOR ( 'NONE', #1442, 1000.000000000000000 ) ;
#7294 = CARTESIAN_POINT ( 'NONE',  ( -30.81806926056963292, 43.62187500034139020, -42.41743335407647209 ) ) ;
#7295 = CARTESIAN_POINT ( 'NONE',  ( -26.02446187185519832, 283.9500510409137632, -4.548923743721432267 ) ) ;
#7296 = ORIENTED_EDGE ( 'NONE', *, *, #7266, .F. ) ;
#7297 = CARTESIAN_POINT ( 'NONE',  ( -40.34137639590981195, 36.12187500034139731, 29.30972558990012189 ) ) ;
#7298 = VERTEX_POINT ( 'NONE', #4653 ) ;
#7299 = ORIENTED_EDGE ( 'NONE', *, *, #4180, .F. ) ;
#7300 = ORIENTED_EDGE ( 'NONE', *, *, #2598, .F. ) ;
#7301 = VECTOR ( 'NONE', #13191, 1000.000000000000000 ) ;
#7302 = CARTESIAN_POINT ( 'NONE',  ( -49.99999999999999289, 39.68125000068280173, -16.24598481164531449 ) ) ;
#7303 = PLANE ( 'NONE',  #14730 ) ;
#7304 = VECTOR ( 'NONE', #4179, 1000.000000000000000 ) ;
#7305 = CARTESIAN_POINT ( 'NONE',  ( -1.240322475938754499E-13, 38.28125000068280315, 50.00000000000000000 ) ) ;
#7306 = DIRECTION ( 'NONE',  ( -0.000000000000000000, 1.000000000000000000, -0.000000000000000000 ) ) ;
#7307 = CARTESIAN_POINT ( 'NONE',  ( 49.86468353124999453, 40.95937500034140299, -16.20201782572376459 ) ) ;
#7308 = CARTESIAN_POINT ( 'NONE',  ( 49.86468353124999453, 42.95937500034139589, -16.20201782572376104 ) ) ;
#7309 = CARTESIAN_POINT ( 'NONE',  ( -3.111920190527341144E-15, 29.50000000000000000, -50.00000000000000000 ) ) ;
#7310 = CARTESIAN_POINT ( 'NONE',  ( 0.000000000000000000, 280.0000000000000000, 88.87749532708107836 ) ) ;
#7311 = FILL_AREA_STYLE ('',( #7224 ) ) ;
#7312 = DIRECTION ( 'NONE',  ( 6.938893903907231459E-18, -1.000000000000000000, -5.551115123125782702E-17 ) ) ;
#7313 = CARTESIAN_POINT ( 'NONE',  ( 3.147895402236133400, 5.285449336779636909, 101.0000000000000000 ) ) ;
#7314 = ORIENTED_EDGE ( 'NONE', *, *, #9863, .T. ) ;
#7315 = CIRCLE ( 'NONE', #8907, 92.05189185291139609 ) ;
#7316 = CARTESIAN_POINT ( 'NONE',  ( -15.40903463028481646, 23.45937500034139944, -47.42413220539093999 ) ) ;
#7317 = VERTEX_POINT ( 'NONE', #13367 ) ;
#7318 = ORIENTED_EDGE ( 'NONE', *, *, #11093, .T. ) ;
#7319 = ORIENTED_EDGE ( 'NONE', *, *, #9318, .T. ) ;
#7320 = CARTESIAN_POINT ( 'NONE',  ( -49.99999999999999289, 41.88125000068279746, 16.24598481164533226 ) ) ;
#7321 = CARTESIAN_POINT ( 'NONE',  ( 50.00000000000000000, 47.00000000000000000, -6.123233995736766085E-15 ) ) ;
#7322 = DIRECTION ( 'NONE',  ( -0.000000000000000000, 1.000000000000000000, -0.000000000000000000 ) ) ;
#7323 = ORIENTED_EDGE ( 'NONE', *, *, #14511, .T. ) ;
#7324 = CARTESIAN_POINT ( 'NONE',  ( 8.446640517145639571E-15, 48.28125000068279604, 50.00000000000000000 ) ) ;
#7325 =( LENGTH_UNIT ( ) NAMED_UNIT ( * ) SI_UNIT ( .MILLI., .METRE. ) );
#7326 = CARTESIAN_POINT ( 'NONE',  ( -17.50000000000000355, 21.92963385674405785, 94.52695465929356544 ) ) ;
#7327 = CARTESIAN_POINT ( 'NONE',  ( -2.500000000000000000, 217.0000000000000284, 44.93050188902856945 ) ) ;
#7328 = DIRECTION ( 'NONE',  ( 1.000000000000000000, 0.000000000000000000, 0.000000000000000000 ) ) ;
#7329 = CIRCLE ( 'NONE', #134, 5.000000000000000888 ) ;
#7330 = EDGE_CURVE ( 'NONE', #9682, #9545, #5223, .T. ) ;
#7331 = CARTESIAN_POINT ( 'NONE',  ( -2.547328955960238000E-13, 32.50000000000000000, 49.99999999999999289 ) ) ;
#7332 = CARTESIAN_POINT ( 'NONE',  ( 50.00000000000000000, 36.78125000068280315, -6.123233995736766085E-15 ) ) ;
#7333 = CARTESIAN_POINT ( 'NONE',  ( -46.19495089481165451, 20.00000000000000355, 18.77607397657153143 ) ) ;
#7334 = FACE_OUTER_BOUND ( 'NONE', #4603, .T. ) ;
#7335 = DIRECTION ( 'NONE',  ( 0.9781476007338041345, 0.2079116908177665313, 0.000000000000000000 ) ) ;
#7336 = CARTESIAN_POINT ( 'NONE',  ( 49.99999999999999289, 27.10000000000000497, -16.24598481164532160 ) ) ;
#7337 = CARTESIAN_POINT ( 'NONE',  ( -49.99999999999999289, 26.10000000000000142, 16.24598481164533226 ) ) ;
#7338 = CARTESIAN_POINT ( 'NONE',  ( -7.919222016226816763, 43.55125428154684641, -49.99999999999999289 ) ) ;
#7339 = EDGE_CURVE ( 'NONE', #11991, #8154, #6980, .T. ) ;
#7340 = EDGE_CURVE ( 'NONE', #6342, #9634, #5734, .T. ) ;
#7341 = CARTESIAN_POINT ( 'NONE',  ( -40.34137639590981195, 48.05937500034139731, 29.30972558990012189 ) ) ;
#7342 = EDGE_LOOP ( 'NONE', ( #9203, #379, #15520 ) ) ;
#7343 = CIRCLE ( 'NONE', #2542, 65.15972704814865324 ) ;
#7344 = TOROIDAL_SURFACE ( 'NONE', #8393, 2.267949192431125027, 2.000000000000000000 ) ;
#7345 = VECTOR ( 'NONE', #350, 1000.000000000000000 ) ;
#7346 = CARTESIAN_POINT ( 'NONE',  ( 4.320770838041294581, 30.97531352606685218, 102.0000000000000142 ) ) ;
#7347 = EDGE_CURVE ( 'NONE', #7211, #10911, #7061, .T. ) ;
#7348 = EDGE_LOOP ( 'NONE', ( #3474, #6782, #4373, #13782 ) ) ;
#7349 = PLANE ( 'NONE',  #14755 ) ;
#7351 =( BOUNDED_CURVE ( )  B_SPLINE_CURVE ( 2, ( #15105, #8790, #9296, #4140, #299, #4227, #221, #11623, #1383, #14350, #2714, #6650, #7958 ),
 .UNSPECIFIED., .F., .F. ) 
 B_SPLINE_CURVE_WITH_KNOTS ( ( 3, 2, 2, 2, 2, 2, 3 ),
 ( 0.4833333333333333370, 0.4866666666666666918, 0.4933333333333333459, 0.5000000000000000000, 0.5066666666666667096, 0.5133333333333333082, 0.5166666666666667185 ),
 .UNSPECIFIED. ) 
 CURVE ( )  GEOMETRIC_REPRESENTATION_ITEM ( )  RATIONAL_B_SPLINE_CURVE ( ( 0.9755282581475768211, 0.9755282581475768211, 1.000000000000000000, 0.9510565162951535312, 1.000000000000000000, 0.9510565162951535312, 1.000000000000000000, 0.9510565162951535312, 1.000000000000000000, 0.9510565162951535312, 1.000000000000000000, 0.9755282581475763770, 0.9755282581475768211 ) ) 
 REPRESENTATION_ITEM ( '' )  );
#7350 = CARTESIAN_POINT ( 'NONE',  ( -40.34137639590981905, 33.65937500034139873, -29.30972558990011478 ) ) ;
#7352 = DIRECTION ( 'NONE',  ( 1.000000000000000000, 0.000000000000000000, 0.000000000000000000 ) ) ;
#7353 = DIRECTION ( 'NONE',  ( 0.000000000000000000, 0.000000000000000000, -1.000000000000000000 ) ) ;
#7354 = CARTESIAN_POINT ( 'NONE',  ( 24.99999999999999645, 287.0000000000000568, 7.500000000000002665 ) ) ;
#7355 = CARTESIAN_POINT ( 'NONE',  ( -3.210462471511496205E-15, 25.42187500034139092, -52.43083105670540789 ) ) ;
#7356 = CARTESIAN_POINT ( 'NONE',  ( 30.81806926056964002, 28.55937500034139376, 42.41743335407646498 ) ) ;
#7357 = VECTOR ( 'NONE', #8504, 1000.000000000000000 ) ;
#7358 = AXIS2_PLACEMENT_3D ( 'NONE', #4170, #6592, #5421 ) ;
#7359 = DIRECTION ( 'NONE',  ( 0.000000000000000000, 1.000000000000000000, 0.000000000000000000 ) ) ;
#7360 = CARTESIAN_POINT ( 'NONE',  ( 30.81806926056964002, 38.62187500034139020, 42.41743335407646498 ) ) ;
#7361 = CIRCLE ( 'NONE', #4176, 45.00000000000000711 ) ;
#7362 = DIRECTION ( 'NONE',  ( 0.1045284632676436315, 0.9945218953682742891, 0.000000000000000000 ) ) ;
#7363 = CARTESIAN_POINT ( 'NONE',  ( -30.81806926056963292, 35.55937500034139020, -42.41743335407647209 ) ) ;
#7364 = CARTESIAN_POINT ( 'NONE',  ( 30.81806926056964002, 40.62187500034139731, 42.41743335407647209 ) ) ;
#7365 = CARTESIAN_POINT ( 'NONE',  ( 40.45084971874737789, 44.79999999999999716, 29.38926261462365375 ) ) ;
#7366 = ORIENTED_EDGE ( 'NONE', *, *, #12974, .T. ) ;
#7367 = CARTESIAN_POINT ( 'NONE',  ( 9.631387414534489405E-15, 44.35937500034140157, 52.43083105670540789 ) ) ;
#7368 = VECTOR ( 'NONE', #6589, 1000.000000000000000 ) ;
#7369 = VERTEX_POINT ( 'NONE', #3310 ) ;
#7371 = CARTESIAN_POINT ( 'NONE',  ( -40.45084971874737789, 27.58125000068280031, -29.38926261462365730 ) ) ;
#7370 = VECTOR ( 'NONE', #4005, 1000.000000000000114 ) ;
#7372 = VERTEX_POINT ( 'NONE', #2060 ) ;
#7373 = DIRECTION ( 'NONE',  ( 0.5877852522924688072, 0.8090169943749505599, 0.000000000000000000 ) ) ;
#7374 = CARTESIAN_POINT ( 'NONE',  ( 40.34137639590981195, 49.12187500034139731, -29.30972558990011834 ) ) ;
#7375 = LINE ( 'NONE', #2036, #8105 ) ;
#7376 = CARTESIAN_POINT ( 'NONE',  ( 30.81806926056964002, 22.62187500034139731, 42.41743335407647209 ) ) ;
#7377 = CARTESIAN_POINT ( 'NONE',  ( 50.00000000000000000, 34.78125000068280315, -6.123233995736766085E-15 ) ) ;
#7378 = CARTESIAN_POINT ( 'NONE',  ( 15.40903463028482356, 36.52187500034139589, 47.42413220539093999 ) ) ;
#7379 = CARTESIAN_POINT ( 'NONE',  ( -26.40559293885987913, 283.2826504366940412, -8.905592938856969454 ) ) ;
#7380 = CARTESIAN_POINT ( 'NONE',  ( 40.34137639590981905, 38.72187500034139873, 29.30972558990010768 ) ) ;
#7381 = CARTESIAN_POINT ( 'NONE',  ( -49.99999999999999289, 31.88125000068280102, 16.24598481164533226 ) ) ;
#7382 = ORIENTED_EDGE ( 'NONE', *, *, #15572, .F. ) ;
#7383 = VERTEX_POINT ( 'NONE', #7149 ) ;
#7384 = CIRCLE ( 'NONE', #8188, 87.81953344283027718 ) ;
#7385 = VERTEX_POINT ( 'NONE', #12210 ) ;
#7386 = EDGE_CURVE ( 'NONE', #172, #16078, #16025, .T. ) ;
#7387 = CARTESIAN_POINT ( 'NONE',  ( 33.58330087751676984, 29.97008732934371622, 22.31061932476934118 ) ) ;
#7388 = CARTESIAN_POINT ( 'NONE',  ( -2.547328955960238000E-13, 34.28125000068279604, 49.99999999999999289 ) ) ;
#7389 = CARTESIAN_POINT ( 'NONE',  ( 7.919222016226822092, 26.55125428154684641, 49.99999999999999289 ) ) ;
#7390 = CARTESIAN_POINT ( 'NONE',  ( -43.87482193696061472, 262.0000000000000000, -10.00000000000000178 ) ) ;
#7391 = CARTESIAN_POINT ( 'NONE',  ( 49.86468353125001585, 38.75937500034139305, 16.20201782572375038 ) ) ;
#7392 = CARTESIAN_POINT ( 'NONE',  ( -15.40903463028481646, 41.45937500034140299, -47.42413220539093999 ) ) ;
#7393 = CARTESIAN_POINT ( 'NONE',  ( -1.224646799147353217E-14, 0.000000000000000000, -100.0000000000000000 ) ) ;
#7394 = PLANE ( 'NONE',  #9401 ) ;
#7395 = CARTESIAN_POINT ( 'NONE',  ( 15.45084971874736723, 41.40000000000000568, -47.55282581475768211 ) ) ;
#7396 = CARTESIAN_POINT ( 'NONE',  ( 1.293669679204937499E-13, 41.50000000000000000, -50.00000000000000000 ) ) ;
#7397 = ORIENTED_EDGE ( 'NONE', *, *, #12457, .T. ) ;
#7398 = CARTESIAN_POINT ( 'NONE',  ( -30.81806926056963292, 25.55937500034139376, -42.41743335407647209 ) ) ;
#7399 = VERTEX_POINT ( 'NONE', #12617 ) ;
#7400 = ORIENTED_EDGE ( 'NONE', *, *, #14008, .F. ) ;
#7401 = ORIENTED_EDGE ( 'NONE', *, *, #12294, .F. ) ;
#7402 = CARTESIAN_POINT ( 'NONE',  ( 40.45084971874737789, 38.58125000068280031, 29.38926261462365375 ) ) ;
#7403 = CARTESIAN_POINT ( 'NONE',  ( -7.919222016226870942, 40.44874571845315359, 49.99999999999997158 ) ) ;
#7404 = CARTESIAN_POINT ( 'NONE',  ( -3.111920190527341144E-15, 29.50000000000000000, -50.00000000000000000 ) ) ;
#7405 = ORIENTED_EDGE ( 'NONE', *, *, #2245, .F. ) ;
#7406 = CARTESIAN_POINT ( 'NONE',  ( 9.657683769731223222, 91.78451504404918637, 2.612942168795361120 ) ) ;
#7407 = DIRECTION ( 'NONE',  ( -0.000000000000000000, 1.000000000000000000, -0.000000000000000000 ) ) ;
#7408 = CARTESIAN_POINT ( 'NONE',  ( -0.5790451294426995910, 4.999999999999993783, 99.11836509645767990 ) ) ;
#7409 = CARTESIAN_POINT ( 'NONE',  ( -6.725310538855818976, 29.22831317314782851, 101.0000000000000000 ) ) ;
#7410 = CARTESIAN_POINT ( 'NONE',  ( 50.00000000000000711, 26.68125000068279462, 16.24598481164530739 ) ) ;
#7411 = DIRECTION ( 'NONE',  ( 0.000000000000000000, 0.000000000000000000, -1.000000000000000000 ) ) ;
#7412 = LINE ( 'NONE', #9119, #707 ) ;
#7413 = CARTESIAN_POINT ( 'NONE',  ( 15.45084971874736723, 49.39999999999999858, -47.55282581475768211 ) ) ;
#7414 = CARTESIAN_POINT ( 'NONE',  ( 40.45084971874737079, 46.98125000068280599, -29.38926261462366440 ) ) ;
#7415 = FACE_OUTER_BOUND ( 'NONE', #4440, .T. ) ;
#7416 = ADVANCED_FACE ( 'NONE', ( #5077 ), #5166, .T. ) ;
#7417 = CARTESIAN_POINT ( 'NONE',  ( -40.45084971874737079, 26.20000000000000284, 29.38926261462367151 ) ) ;
#7418 = CARTESIAN_POINT ( 'NONE',  ( 40.34137639590981905, 22.65937500034139518, 29.30972558990010768 ) ) ;
#7419 = CARTESIAN_POINT ( 'NONE',  ( -30.90169943749473447, 42.08125000068279320, 42.53254041760200721 ) ) ;
#7420 = CARTESIAN_POINT ( 'NONE',  ( -49.86468353124999453, 43.95937500034138878, 16.20201782572377525 ) ) ;
#7421 = ORIENTED_EDGE ( 'NONE', *, *, #11209, .T. ) ;
#7422 = CARTESIAN_POINT ( 'NONE',  ( -15.40903463028480580, 26.25937500034140015, 47.42413220539094709 ) ) ;
#7423 = VERTEX_POINT ( 'NONE', #2467 ) ;
#7424 = CARTESIAN_POINT ( 'NONE',  ( 40.45084971874737079, 49.20000000000000284, -29.38926261462366440 ) ) ;
#7425 = CARTESIAN_POINT ( 'NONE',  ( -3.210462471511496205E-15, 37.35937500034139447, -52.43083105670540789 ) ) ;
#7426 = DIRECTION ( 'NONE',  ( 0.000000000000000000, 1.000000000000000000, 0.000000000000000000 ) ) ;
#7428 = EDGE_CURVE ( 'NONE', #9397, #1352, #87, .T. ) ;
#7427 = CARTESIAN_POINT ( 'NONE',  ( -40.45084971874737789, 49.58125000068280031, -29.38926261462365730 ) ) ;
#7429 = CARTESIAN_POINT ( 'NONE',  ( 46.13167797950631410, 24.99999999999999289, -18.93026546213357619 ) ) ;
#7430 = ADVANCED_BREP_SHAPE_REPRESENTATION ( '', ( #3187, #15812 ), #9193 ) ;
#7431 = STYLED_ITEM ( 'NONE', ( #16272 ), #3187 ) ;
#7432 = CARTESIAN_POINT ( 'NONE',  ( -15.40903463028480580, 22.32187500034139660, 47.42413220539094709 ) ) ;
#7433 = CARTESIAN_POINT ( 'NONE',  ( 49.86468353125000164, 30.85937500034139802, -6.106662507704105588E-15 ) ) ;
#7434 = CARTESIAN_POINT ( 'NONE',  ( 15.45084971874737789, 26.38125000068280102, 47.55282581475767500 ) ) ;
#7435 = CARTESIAN_POINT ( 'NONE',  ( -49.86468353124999453, 36.02187500034139589, 16.20201782572377169 ) ) ;
#7436 = DIRECTION ( 'NONE',  ( -0.000000000000000000, 1.000000000000000000, -0.000000000000000000 ) ) ;
#7437 = ADVANCED_FACE ( 'NONE', ( #10130 ), #11454, .T. ) ;
#7438 = CARTESIAN_POINT ( 'NONE',  ( -15.45084971874737256, 37.60000000000000142, -47.55282581475767500 ) ) ;
#7439 = CARTESIAN_POINT ( 'NONE',  ( 30.81806926056964002, 40.55937500034139731, 42.41743335407647209 ) ) ;
#7440 = CARTESIAN_POINT ( 'NONE',  ( -49.86468353124999453, 40.02187500034140299, 16.20201782572377525 ) ) ;
#7441 = CARTESIAN_POINT ( 'NONE',  ( 15.45084971874736723, 43.39999999999999858, -47.55282581475768211 ) ) ;
#7443 = ORIENTED_EDGE ( 'NONE', *, *, #14840, .F. ) ;
#7442 =( BOUNDED_CURVE ( )  B_SPLINE_CURVE ( 3, ( #3802, #6139, #7387, #42 ),
 .UNSPECIFIED., .F., .F. ) 
 B_SPLINE_CURVE_WITH_KNOTS ( ( 4, 4 ),
 ( 4.523772594209285458, 4.901005366560093002 ),
 .UNSPECIFIED. ) 
 CURVE ( )  GEOMETRIC_REPRESENTATION_ITEM ( )  RATIONAL_B_SPLINE_CURVE ( ( 1.000000000000000000, 0.9881764018959044993, 0.9881764018959044993, 1.000000000000000000 ) ) 
 REPRESENTATION_ITEM ( '' )  );
#7444 = EDGE_CURVE ( 'NONE', #4152, #646, #50, .T. ) ;
#7445 = CARTESIAN_POINT ( 'NONE',  ( -15.40903463028480580, 44.25937500034140015, 47.42413220539094709 ) ) ;
#7446 = ORIENTED_EDGE ( 'NONE', *, *, #15400, .F. ) ;
#7447 = CARTESIAN_POINT ( 'NONE',  ( 15.45084971874736723, 25.18125000068279817, -47.55282581475768211 ) ) ;
#7448 = DIRECTION ( 'NONE',  ( 0.000000000000000000, -0.000000000000000000, 1.000000000000000000 ) ) ;
#7449 = DIRECTION ( 'NONE',  ( 6.938893903907231459E-18, -1.000000000000000000, -5.551115123125782702E-17 ) ) ;
#7450 = CARTESIAN_POINT ( 'NONE',  ( 40.34137639590981905, 40.72187500034139873, 29.30972558990010768 ) ) ;
#7451 = CARTESIAN_POINT ( 'NONE',  ( 30.90169943749475223, 30.70000000000000284, 42.53254041760199300 ) ) ;
#7452 = CARTESIAN_POINT ( 'NONE',  ( 30.81806926056962936, 21.22187500034139518, -42.41743335407647209 ) ) ;
#7453 = EDGE_CURVE ( 'NONE', #13275, #2321, #6260, .T. ) ;
#7454 = CARTESIAN_POINT ( 'NONE',  ( -40.45084971874737079, 27.98125000068279888, 29.38926261462367151 ) ) ;
#7455 = CARTESIAN_POINT ( 'NONE',  ( -40.34137639590981195, 36.12187500034139731, 29.30972558990012189 ) ) ;
#7456 = CARTESIAN_POINT ( 'NONE',  ( -23.39173249367811636, 283.2330659413073590, -9.195866246827240076 ) ) ;
#7457 = CARTESIAN_POINT ( 'NONE',  ( -30.81806926056963292, 37.62187500034139020, -42.41743335407647209 ) ) ;
#7458 = CARTESIAN_POINT ( 'NONE',  ( -49.99999999999999289, 41.88125000068279746, 16.24598481164533226 ) ) ;
#7459 = ORIENTED_EDGE ( 'NONE', *, *, #6127, .T. ) ;
#7460 = ORIENTED_EDGE ( 'NONE', *, *, #12461, .F. ) ;
#7461 = VERTEX_POINT ( 'NONE', #6393 ) ;
#7462 = DIRECTION ( 'NONE',  ( 1.000000000000000000, 0.000000000000000000, 0.000000000000000000 ) ) ;
#7463 = CARTESIAN_POINT ( 'NONE',  ( 16.78599477205478863, 21.23847499609146183, 101.6666710451724214 ) ) ;
#7464 = CARTESIAN_POINT ( 'NONE',  ( -40.45084971874737789, 21.58125000068279675, -29.38926261462365730 ) ) ;
#7465 = CARTESIAN_POINT ( 'NONE',  ( 8.880528407616436581, 25.91118970470966687, 101.0000000000000000 ) ) ;
#7466 = CARTESIAN_POINT ( 'NONE',  ( 15.40903463028482356, 30.45937500034139589, 47.42413220539093999 ) ) ;
#7467 = ADVANCED_FACE ( 'NONE', ( #5153 ), #7394, .T. ) ;
#7468 = CARTESIAN_POINT ( 'NONE',  ( 0.000000000000000000, 272.0000000000000000, 0.000000000000000000 ) ) ;
#7469 = DIRECTION ( 'NONE',  ( -0.7431448254773860285, -0.6691306063588672304, 0.000000000000000000 ) ) ;
#7470 = CARTESIAN_POINT ( 'NONE',  ( -7.732050807568878525, 22.50000000000000000, 100.0000000000000000 ) ) ;
#7471 = CARTESIAN_POINT ( 'NONE',  ( 0.000000000000000000, 25.00000000000000355, 0.000000000000000000 ) ) ;
#7472 = ORIENTED_EDGE ( 'NONE', *, *, #12231, .F. ) ;
#7473 = CARTESIAN_POINT ( 'NONE',  ( 15.40903463028481113, 25.25937500034139660, -47.42413220539094709 ) ) ;
#7474 = ORIENTED_EDGE ( 'NONE', *, *, #13332, .T. ) ;
#7475 = ORIENTED_EDGE ( 'NONE', *, *, #1229, .T. ) ;
#7476 = CARTESIAN_POINT ( 'NONE',  ( 50.00000000000000711, 38.68125000068280173, 16.24598481164530739 ) ) ;
#7477 = DIRECTION ( 'NONE',  ( 0.000000000000000000, 0.000000000000000000, -1.000000000000000000 ) ) ;
#7478 = DIRECTION ( 'NONE',  ( 1.000000000000000000, 0.000000000000000000, 0.000000000000000000 ) ) ;
#7479 = ORIENTED_EDGE ( 'NONE', *, *, #1871, .F. ) ;
#7480 = DIRECTION ( 'NONE',  ( -0.000000000000000000, 1.000000000000000000, -0.000000000000000000 ) ) ;
#7481 = CARTESIAN_POINT ( 'NONE',  ( -20.00000000000000355, 287.0000000000000568, -2.499999999999998668 ) ) ;
#7482 = CARTESIAN_POINT ( 'NONE',  ( 40.45084971874737079, 32.98125000068279888, -29.38926261462366440 ) ) ;
#7483 = CARTESIAN_POINT ( 'NONE',  ( -7.500000000000005329, 25.00000000000000355, 24.29058411375428506 ) ) ;
#7484 = CARTESIAN_POINT ( 'NONE',  ( -9.500222237632405253, 22.00424054664139817, 101.0000000000000000 ) ) ;
#7485 = DIRECTION ( 'NONE',  ( -0.4067366430757887175, -0.9135454576426059736, 0.000000000000000000 ) ) ;
#7486 =( NAMED_UNIT ( * ) PLANE_ANGLE_UNIT ( ) SI_UNIT ( $, .RADIAN. ) );
#7487 = CARTESIAN_POINT ( 'NONE',  ( -17.28626291527383785, 40.00000000000000711, 18.64048258526051427 ) ) ;
#7488 = CARTESIAN_POINT ( 'NONE',  ( -30.90169943749473802, 48.08125000068278609, 42.53254041760200721 ) ) ;
#7489 = CARTESIAN_POINT ( 'NONE',  ( 6.386939227490392668, 38.07459704542245049, 101.6666710451724214 ) ) ;
#7490 = CARTESIAN_POINT ( 'NONE',  ( -30.90169943749473802, 22.30000000000000071, 42.53254041760200721 ) ) ;
#7491 = CARTESIAN_POINT ( 'NONE',  ( -15.40903463028480580, 20.25937500034139660, 47.42413220539094709 ) ) ;
#7492 = CARTESIAN_POINT ( 'NONE',  ( 0.000000000000000000, 102.0000000000000142, -5.000000000000000000 ) ) ;
#7493 = CARTESIAN_POINT ( 'NONE',  ( 49.86468353125000164, 42.85937500034140157, -6.106662507704105588E-15 ) ) ;
#7494 = VERTEX_POINT ( 'NONE', #8964 ) ;
#7495 = CARTESIAN_POINT ( 'NONE',  ( 7.513064459987437071E-14, 42.28125000068280315, 50.00000000000000000 ) ) ;
#7496 = EDGE_LOOP ( 'NONE', ( #4554, #6527, #3977, #5703 ) ) ;
#7497 = LINE ( 'NONE', #7576, #2835 ) ;
#7498 = CARTESIAN_POINT ( 'NONE',  ( -3.210462471511496205E-15, 29.35937500034139802, -52.43083105670540789 ) ) ;
#7499 =( BOUNDED_CURVE ( )  B_SPLINE_CURVE ( 2, ( #7657, #1498, #3753, #12727, #11475, #10233, #15292, #10720, #12975, #7980, #5507, #400, #9146 ),
 .UNSPECIFIED., .F., .T. ) 
 B_SPLINE_CURVE_WITH_KNOTS ( ( 3, 2, 2, 2, 2, 2, 3 ),
 ( 0.08333333333333334259, 0.08666666666666666963, 0.09333333333333333759, 0.1000000000000000056, 0.1066666666666666735, 0.1133333333333333276, 0.1166666666666666685 ),
 .UNSPECIFIED. ) 
 CURVE ( )  GEOMETRIC_REPRESENTATION_ITEM ( )  RATIONAL_B_SPLINE_CURVE ( ( 0.9755282581475768211, 0.9755282581475768211, 1.000000000000000000, 0.9510565162951535312, 1.000000000000000000, 0.9510565162951535312, 1.000000000000000000, 0.9510565162951535312, 1.000000000000000000, 0.9510565162951535312, 1.000000000000000000, 0.9755282581475767101, 0.9755282581475768211 ) ) 
 REPRESENTATION_ITEM ( '' )  );
#7500 = DIRECTION ( 'NONE',  ( 0.000000000000000000, -1.000000000000000000, -0.000000000000000000 ) ) ;
#7501 = CARTESIAN_POINT ( 'NONE',  ( 45.60931600130358987, 25.00000000000000000, -20.15700215907558146 ) ) ;
#7502 = CARTESIAN_POINT ( 'NONE',  ( 40.45084971874737789, 46.58125000068280031, 29.38926261462365375 ) ) ;
#7503 = CARTESIAN_POINT ( 'NONE',  ( -40.34137639590981905, 21.72187500034139518, -29.30972558990011478 ) ) ;
#7504 = CARTESIAN_POINT ( 'NONE',  ( -49.86468353125000164, 23.85937500034139447, 0.000000000000000000 ) ) ;
#7505 = CARTESIAN_POINT ( 'NONE',  ( -3.111920190527341144E-15, 43.50000000000000711, -50.00000000000000000 ) ) ;
#7506 = CARTESIAN_POINT ( 'NONE',  ( 15.40903463028481113, 35.32187500034139305, -47.42413220539094709 ) ) ;
#7507 = CARTESIAN_POINT ( 'NONE',  ( 9.189545401991395579, 24.96013318841451678, 101.0000000000000000 ) ) ;
#7508 = CARTESIAN_POINT ( 'NONE',  ( 50.00000000000000711, 38.89999999999999858, 16.24598481164530739 ) ) ;
#7509 = CARTESIAN_POINT ( 'NONE',  ( -30.81806926056963292, 39.55937500034139731, -42.41743335407647209 ) ) ;
#7510 = CARTESIAN_POINT ( 'NONE',  ( 30.81806926056962936, 33.22187500034139163, -42.41743335407647209 ) ) ;
#7511 = VECTOR ( 'NONE', #2716, 1000.000000000000000 ) ;
#7512 = B_SPLINE_CURVE_WITH_KNOTS ( 'NONE', 3,
 ( #10953, #15938, #2207, #5806 ),
 .UNSPECIFIED., .F., .F.,
 ( 4, 4 ),
 ( 2.829004760702349710E-07, 0.001414802801989369606 ),
 .UNSPECIFIED. ) ;
#7513 = CARTESIAN_POINT ( 'NONE',  ( -49.99999999999999289, 47.89999999999999858, -16.24598481164531449 ) ) ;
#7514 = EDGE_LOOP ( 'NONE', ( #7397, #11144, #13622, #15005 ) ) ;
#7515 = CARTESIAN_POINT ( 'NONE',  ( 49.86468353125000164, 34.85937500034140157, -6.106662507704105588E-15 ) ) ;
#7516 = ORIENTED_EDGE ( 'NONE', *, *, #5772, .F. ) ;
#7517 = ORIENTED_EDGE ( 'NONE', *, *, #1432, .T. ) ;
#7518 = CARTESIAN_POINT ( 'NONE',  ( 30.90169943749474157, 27.08125000068280031, -42.53254041760200721 ) ) ;
#7519 = CARTESIAN_POINT ( 'NONE',  ( -1.240322475938754499E-13, 40.28125000068280315, 50.00000000000000000 ) ) ;
#7520 = CARTESIAN_POINT ( 'NONE',  ( 49.86468353125001585, 26.82187500034138949, 16.20201782572375038 ) ) ;
#7521 = VECTOR ( 'NONE', #7267, 999.9999999999998863 ) ;
#7522 = DIRECTION ( 'NONE',  ( -1.000000000000000000, 0.000000000000000000, 1.734723475976807094E-17 ) ) ;
#7523 = CARTESIAN_POINT ( 'NONE',  ( 40.34137639590981905, 42.72187500034139873, 29.30972558990010768 ) ) ;
#7524 = CARTESIAN_POINT ( 'NONE',  ( -15.45084971874737256, 25.38125000068279746, -47.55282581475767500 ) ) ;
#7525 = EDGE_CURVE ( 'NONE', #14047, #15954, #14020, .T. ) ;
#7526 = CARTESIAN_POINT ( 'NONE',  ( 40.45084971874737789, 46.80000000000000426, 29.38926261462365375 ) ) ;
#7527 = CARTESIAN_POINT ( 'NONE',  ( 50.00000000000000711, 30.68125000068279462, 16.24598481164530739 ) ) ;
#7528 = CARTESIAN_POINT ( 'NONE',  ( 5.648665123217551098, 39.07342515812086248, 92.94044983197015597 ) ) ;
#7529 =( BOUNDED_CURVE ( )  B_SPLINE_CURVE ( 3, ( #948, #784, #6129, #16251 ),
 .UNSPECIFIED., .F., .F. ) 
 B_SPLINE_CURVE_WITH_KNOTS ( ( 4, 4 ),
 ( 5.700094519411438299, 6.866276094947727948 ),
 .UNSPECIFIED. ) 
 CURVE ( )  GEOMETRIC_REPRESENTATION_ITEM ( )  RATIONAL_B_SPLINE_CURVE ( ( 1.000000000000000000, 0.8898432210558864242, 0.8898432210558864242, 1.000000000000000000 ) ) 
 REPRESENTATION_ITEM ( '' )  );
#7530 = ADVANCED_FACE ( 'NONE', ( #1054 ), #3654, .T. ) ;
#7531 = CARTESIAN_POINT ( 'NONE',  ( -15.40903463028480580, 36.32187500034140015, 47.42413220539094709 ) ) ;
#7532 = CARTESIAN_POINT ( 'NONE',  ( -26.77784341583514305, 282.2553694771637538, -10.88892170791705105 ) ) ;
#7533 = EDGE_CURVE ( 'NONE', #1181, #5830, #1426, .T. ) ;
#7534 = VECTOR ( 'NONE', #5092, 1000.000000000000000 ) ;
#7535 = CARTESIAN_POINT ( 'NONE',  ( -30.81806926056962226, 38.22187500034139873, 42.41743335407647919 ) ) ;
#7536 = LINE ( 'NONE', #10040, #7863 ) ;
#7537 = ORIENTED_EDGE ( 'NONE', *, *, #10707, .F. ) ;
#7538 = EDGE_CURVE ( 'NONE', #6674, #14577, #14967, .T. ) ;
#7539 = ORIENTED_EDGE ( 'NONE', *, *, #16267, .F. ) ;
#7540 = LINE ( 'NONE', #15174, #2041 ) ;
#7541 = CARTESIAN_POINT ( 'NONE',  ( 0.000000000000000000, 22.50000000000000000, 102.0000000000000142 ) ) ;
#7542 = CARTESIAN_POINT ( 'NONE',  ( 9.735664389687646693E-15, 272.0000000000000000, -79.49773270518484480 ) ) ;
#7543 = DIRECTION ( 'NONE',  ( 0.000000000000000000, 1.000000000000000000, 0.000000000000000000 ) ) ;
#7544 = CARTESIAN_POINT ( 'NONE',  ( 49.86468353124999453, 28.95937500034139944, -16.20201782572376459 ) ) ;
#7545 =( NAMED_UNIT ( * ) PLANE_ANGLE_UNIT ( ) SI_UNIT ( $, .RADIAN. ) );
#7546 = AXIS2_PLACEMENT_3D ( 'NONE', #3402, #9806, #5980 ) ;
#7547 = CARTESIAN_POINT ( 'NONE',  ( -49.86468353124999453, 46.02187500034139589, 16.20201782572377169 ) ) ;
#7548 = CARTESIAN_POINT ( 'NONE',  ( -40.45084971874737079, 40.20000000000000284, 29.38926261462367151 ) ) ;
#7549 = CYLINDRICAL_SURFACE ( 'NONE', #5290, 50.00000000000000000 ) ;
#7550 = CARTESIAN_POINT ( 'NONE',  ( -7.919222016226752814, 41.55125428154683931, -50.00000000000000711 ) ) ;
#7551 = VERTEX_POINT ( 'NONE', #6225 ) ;
#7552 = CARTESIAN_POINT ( 'NONE',  ( 40.34137639590981195, 23.05937500034139731, -29.30972558990011834 ) ) ;
#7553 = ORIENTED_EDGE ( 'NONE', *, *, #9270, .F. ) ;
#7554 = EDGE_LOOP ( 'NONE', ( #780, #876 ) ) ;
#7555 = ORIENTED_EDGE ( 'NONE', *, *, #1717, .T. ) ;
#7556 = ORIENTED_EDGE ( 'NONE', *, *, #13811, .F. ) ;
#7557 = EDGE_CURVE ( 'NONE', #3318, #6257, #9963, .T. ) ;
#7558 = VECTOR ( 'NONE', #10603, 1000.000000000000000 ) ;
#7559 = DIRECTION ( 'NONE',  ( 0.000000000000000000, 1.000000000000000000, 0.000000000000000000 ) ) ;
#7560 = EDGE_CURVE ( 'NONE', #4580, #6385, #8348, .T. ) ;
#7561 = CARTESIAN_POINT ( 'NONE',  ( -25.00000000000000355, 287.0000000000000568, 7.500000000000001776 ) ) ;
#7562 = CARTESIAN_POINT ( 'NONE',  ( -49.99999999999999289, 38.10000000000000142, 16.24598481164533226 ) ) ;
#7563 = CARTESIAN_POINT ( 'NONE',  ( 40.45084971874737789, 32.58125000068280031, 29.38926261462365375 ) ) ;
#7564 = DIRECTION ( 'NONE',  ( 0.000000000000000000, 1.000000000000000000, 0.000000000000000000 ) ) ;
#7565 = CARTESIAN_POINT ( 'NONE',  ( 15.45084971874736723, 25.18125000068279817, -47.55282581475768211 ) ) ;
#7566 = CARTESIAN_POINT ( 'NONE',  ( 4.898587196589413026E-15, 267.0000000000000000, 40.00000000000000000 ) ) ;
#7567 = LINE ( 'NONE', #3830, #1159 ) ;
#7568 = CARTESIAN_POINT ( 'NONE',  ( -49.99999999999999289, 45.88125000068279746, 16.24598481164533226 ) ) ;
#7569 = CARTESIAN_POINT ( 'NONE',  ( 30.90169943749473802, 21.30000000000000426, -42.53254041760200721 ) ) ;
#7570 = CARTESIAN_POINT ( 'NONE',  ( -30.90169943749474868, 21.69999999999999574, -42.53254041760200721 ) ) ;
#7571 = CARTESIAN_POINT ( 'NONE',  ( -3.111920190527341144E-15, 25.50000000000000355, -50.00000000000000000 ) ) ;
#7572 = CARTESIAN_POINT ( 'NONE',  ( 0.000000000000000000, 22.50000000000000000, 101.0000000000000000 ) ) ;
#7573 = CARTESIAN_POINT ( 'NONE',  ( -15.40903463028480580, 42.25937500034139305, 47.42413220539094709 ) ) ;
#7574 = ORIENTED_EDGE ( 'NONE', *, *, #8290, .T. ) ;
#7575 = ORIENTED_EDGE ( 'NONE', *, *, #3392, .F. ) ;
#7576 = CARTESIAN_POINT ( 'NONE',  ( -17.28626291527383785, 25.00000000000000355, 18.64048258526051427 ) ) ;
#7577 = CARTESIAN_POINT ( 'NONE',  ( 40.34137639590981195, 27.05937500034139731, -29.30972558990011834 ) ) ;
#7579 = EDGE_CURVE ( 'NONE', #8369, #9685, #7351, .T. ) ;
#7578 = VECTOR ( 'NONE', #8460, 1000.000000000000000 ) ;
#7580 = ADVANCED_FACE ( 'NONE', ( #7793 ), #5326, .F. ) ;
#7581 = CARTESIAN_POINT ( 'NONE',  ( 30.90169943749473802, 33.30000000000000426, -42.53254041760200721 ) ) ;
#7582 = CYLINDRICAL_SURFACE ( 'NONE', #8122, 40.00000000000000000 ) ;
#7583 = STYLED_ITEM ( 'NONE', ( #1074 ), #3231 ) ;
#7584 = CARTESIAN_POINT ( 'NONE',  ( 48.34710198928263480, 25.00000000000000000, -12.20844498793593580 ) ) ;
#7585 = CARTESIAN_POINT ( 'NONE',  ( 49.86468353125000164, 32.92187500034139447, -6.106662507704105588E-15 ) ) ;
#7586 = CARTESIAN_POINT ( 'NONE',  ( 15.45084971874736723, 31.18125000068279817, -47.55282581475768211 ) ) ;
#7587 = CARTESIAN_POINT ( 'NONE',  ( -30.81806926056962226, 20.15937500034140228, 42.41743335407647209 ) ) ;
#7588 = CARTESIAN_POINT ( 'NONE',  ( 50.00000000000000711, 42.89999999999999147, 16.24598481164530739 ) ) ;
#7589 = CARTESIAN_POINT ( 'NONE',  ( 49.86468353125000164, 32.92187500034139447, -6.106662507704105588E-15 ) ) ;
#7590 = CARTESIAN_POINT ( 'NONE',  ( 0.000000000000000000, 52.00000000000000711, 0.000000000000000000 ) ) ;
#7591 = CARTESIAN_POINT ( 'NONE',  ( 49.99999999999999289, 33.10000000000000853, -16.24598481164532160 ) ) ;
#7592 = CARTESIAN_POINT ( 'NONE',  ( 49.86468353124999453, 36.95937500034139589, -16.20201782572376459 ) ) ;
#7593 = AXIS2_PLACEMENT_3D ( 'NONE', #11374, #5237, #7706 ) ;
#7594 = CARTESIAN_POINT ( 'NONE',  ( -49.86468353124999453, 31.82187500034139305, -16.20201782572375393 ) ) ;
#7595 = VECTOR ( 'NONE', #8954, 1000.000000000000114 ) ;
#7596 = AXIS2_PLACEMENT_3D ( 'NONE', #8665, #16312, #13810 ) ;
#7597 = CARTESIAN_POINT ( 'NONE',  ( -40.45084971874737079, 42.20000000000000284, 29.38926261462367151 ) ) ;
#7598 = ORIENTED_EDGE ( 'NONE', *, *, #5256, .T. ) ;
#7599 = CARTESIAN_POINT ( 'NONE',  ( -7.919222016226804328, 26.44874571845315359, 50.00000000000000000 ) ) ;
#7600 = ORIENTED_EDGE ( 'NONE', *, *, #15947, .F. ) ;
#7601 = CARTESIAN_POINT ( 'NONE',  ( 40.34137639590981905, 36.65937500034139873, 29.30972558990010768 ) ) ;
#7602 = VECTOR ( 'NONE', #15665, 1000.000000000000000 ) ;
#7603 = EDGE_LOOP ( 'NONE', ( #9359, #3230 ) ) ;
#7604 = CARTESIAN_POINT ( 'NONE',  ( 43.87482193696061472, 267.0000000000000000, -10.00000000000000000 ) ) ;
#7605 = CARTESIAN_POINT ( 'NONE',  ( 40.34137639590981905, 46.65937500034139873, 29.30972558990010768 ) ) ;
#7606 = CLOSED_SHELL ( 'NONE', ( #6835, #7633, #15971, #15864, #14832, #6124, #12084, #4618, #1329, #846, #1938, #12715, #15846, #9516, #13472, #7027, #6723, #2522, #12585, #3172, #630, #4592, #9583, #14095, #11016, #10190, #12521, #6050, #5793, #2602, #14940, #4707, #14213, #4513, #785, #13614, #13408, #15263, #15776, #7823, #2584, #10328 ) ) ;
#7607 = CARTESIAN_POINT ( 'NONE',  ( -21.39877161664088234, 15.54711762656345897, 101.0000000000000000 ) ) ;
#7608 = VECTOR ( 'NONE', #1750, 1000.000000000000000 ) ;
#7609 = CARTESIAN_POINT ( 'NONE',  ( -49.86468353124999453, 24.02187500034139589, 16.20201782572377525 ) ) ;
#7610 = AXIS2_PLACEMENT_3D ( 'NONE', #5611, #8087, #11918 ) ;
#7611 = DIRECTION ( 'NONE',  ( -0.9135454576426004225, -0.4067366430758009854, 0.000000000000000000 ) ) ;
#7612 = CARTESIAN_POINT ( 'NONE',  ( -15.40903463028481646, 45.52187500034139589, -47.42413220539093999 ) ) ;
#7613 = CARTESIAN_POINT ( 'NONE',  ( -15.45084971874736368, 26.18125000068280173, 47.55282581475768211 ) ) ;
#7614 = CARTESIAN_POINT ( 'NONE',  ( -49.99999999999999289, 49.89999999999999147, -16.24598481164531449 ) ) ;
#7615 = CARTESIAN_POINT ( 'NONE',  ( 49.99999999999999289, 26.88125000068280102, -16.24598481164532160 ) ) ;
#7616 = CARTESIAN_POINT ( 'NONE',  ( -15.40903463028481646, 47.52187500034139589, -47.42413220539093999 ) ) ;
#7617 = CARTESIAN_POINT ( 'NONE',  ( 15.40903463028481113, 33.32187500034139305, -47.42413220539094709 ) ) ;
#7618 = AXIS2_PLACEMENT_3D ( 'NONE', #6515, #8830, #7752 ) ;
#7619 = DIRECTION ( 'NONE',  ( 0.000000000000000000, -0.000000000000000000, 1.000000000000000000 ) ) ;
#7620 = AXIS2_PLACEMENT_3D ( 'NONE', #9816, #11151, #14867 ) ;
#7621 = LINE ( 'NONE', #3957, #3031 ) ;
#7622 = ORIENTED_EDGE ( 'NONE', *, *, #3465, .T. ) ;
#7623 = ORIENTED_EDGE ( 'NONE', *, *, #11598, .T. ) ;
#7624 = DIRECTION ( 'NONE',  ( 0.000000000000000000, -1.000000000000000000, 0.000000000000000000 ) ) ;
#7625 = DIRECTION ( 'NONE',  ( -1.000000000000000000, 0.000000000000000000, -2.312964634635741971E-16 ) ) ;
#7626 = CYLINDRICAL_SURFACE ( 'NONE', #4958, 14.08089297201391155 ) ;
#7627 = CYLINDRICAL_SURFACE ( 'NONE', #6613, 50.00000000000000000 ) ;
#7628 = AXIS2_PLACEMENT_3D ( 'NONE', #10986, #13633, #2243 ) ;
#7629 = CARTESIAN_POINT ( 'NONE',  ( 40.34137639590981905, 28.65937500034139873, 29.30972558990010768 ) ) ;
#7630 = PRESENTATION_STYLE_ASSIGNMENT (( #6390 ) ) ;
#7633 = ADVANCED_FACE ( 'NONE', ( #10376 ), #15433, .F. ) ;
#7632 =( BOUNDED_CURVE ( )  B_SPLINE_CURVE ( 2, ( #11262, #8917, #7676, #16320, #4955, #5118, #10016, #12747, #16410, #5196, #15070, #6271, #3699 ),
 .UNSPECIFIED., .F., .T. ) 
 B_SPLINE_CURVE_WITH_KNOTS ( ( 3, 2, 2, 2, 2, 2, 3 ),
 ( 0.6500000000000000222, 0.6533333333333333215, 0.6600000000000000311, 0.6666666666666666297, 0.6733333333333333393, 0.6800000000000000488, 0.6833333333333333481 ),
 .UNSPECIFIED. ) 
 CURVE ( )  GEOMETRIC_REPRESENTATION_ITEM ( )  RATIONAL_B_SPLINE_CURVE ( ( 0.9755282581475768211, 0.9755282581475771542, 1.000000000000000000, 0.9510565162951535312, 1.000000000000000000, 0.9510565162951535312, 1.000000000000000000, 0.9510565162951535312, 1.000000000000000000, 0.9510565162951535312, 1.000000000000000000, 0.9755282581475768211, 0.9755282581475768211 ) ) 
 REPRESENTATION_ITEM ( '' )  );
#7631 = AXIS2_PLACEMENT_3D ( 'NONE', #7886, #550, #230 ) ;
#7634 = CARTESIAN_POINT ( 'NONE',  ( -40.34137639590981905, 43.72187500034139873, -29.30972558990011478 ) ) ;
#7635 = DIRECTION ( 'NONE',  ( 1.000000000000000000, 0.000000000000000000, 0.000000000000000000 ) ) ;
#7636 = DIRECTION ( 'NONE',  ( -0.000000000000000000, -0.000000000000000000, -1.000000000000000000 ) ) ;
#7637 = CARTESIAN_POINT ( 'NONE',  ( -20.00000000000000355, 307.0000000000000568, 2.500000000000001332 ) ) ;
#7638 = ADVANCED_FACE ( 'NONE', ( #14183 ), #4053, .T. ) ;
#7639 = CARTESIAN_POINT ( 'NONE',  ( -20.00000000000000355, 287.0000000000000568, 7.500000000000001776 ) ) ;
#7640 = VERTEX_POINT ( 'NONE', #14268 ) ;
#7641 = CARTESIAN_POINT ( 'NONE',  ( 15.40903463028482356, 26.45937500034139589, 47.42413220539093999 ) ) ;
#7642 = ORIENTED_EDGE ( 'NONE', *, *, #8744, .F. ) ;
#7643 = CARTESIAN_POINT ( 'NONE',  ( -8.477241335952138357, 18.18301270189218855, 101.0000000000000000 ) ) ;
#7644 = ORIENTED_EDGE ( 'NONE', *, *, #3672, .T. ) ;
#7645 = ORIENTED_EDGE ( 'NONE', *, *, #15916, .F. ) ;
#7646 = EDGE_CURVE ( 'NONE', #11207, #1716, #5244, .T. ) ;
#7647 = CARTESIAN_POINT ( 'NONE',  ( 50.00000000000000000, 34.78125000068280315, -6.123233995736766085E-15 ) ) ;
#7648 = DIRECTION ( 'NONE',  ( -0.000000000000000000, -1.000000000000000000, -0.000000000000000000 ) ) ;
#7649 = CARTESIAN_POINT ( 'NONE',  ( -3.111920190527341144E-15, 27.50000000000000000, -50.00000000000000000 ) ) ;
#7650 = CARTESIAN_POINT ( 'NONE',  ( 9.735664389687646693E-15, 252.1309828287255357, -79.49773270518484480 ) ) ;
#7651 = DIRECTION ( 'NONE',  ( 0.000000000000000000, 0.000000000000000000, -1.000000000000000000 ) ) ;
#7652 = LINE ( 'NONE', #6242, #15489 ) ;
#7653 = CYLINDRICAL_SURFACE ( 'NONE', #4490, 5.000000000000000000 ) ;
#7654 = DIRECTION ( 'NONE',  ( 0.000000000000000000, 0.000000000000000000, -1.000000000000000000 ) ) ;
#7655 = CARTESIAN_POINT ( 'NONE',  ( -49.99999999999999289, 41.68125000068280173, -16.24598481164531449 ) ) ;
#7656 = CARTESIAN_POINT ( 'NONE',  ( -20.00000000000000355, 312.0000000000000568, 7.500000000000001776 ) ) ;
#7657 = CARTESIAN_POINT ( 'NONE',  ( 2.978552182361884590E-14, 47.28125000068279604, -50.00000000000000000 ) ) ;
#7658 = CARTESIAN_POINT ( 'NONE',  ( 8.446640517145639571E-15, 26.50000000000000000, 50.00000000000000000 ) ) ;
#7659 = ORIENTED_EDGE ( 'NONE', *, *, #3464, .T. ) ;
#7660 = CARTESIAN_POINT ( 'NONE',  ( 49.86468353125000164, 46.85937500034139447, -6.106662507704105588E-15 ) ) ;
#7661 = ORIENTED_EDGE ( 'NONE', *, *, #15404, .F. ) ;
#7662 = EDGE_CURVE ( 'NONE', #1769, #5969, #15353, .T. ) ;
#7663 = CARTESIAN_POINT ( 'NONE',  ( 30.90169943749473802, 43.08125000068280031, -42.53254041760200721 ) ) ;
#7664 = AXIS2_PLACEMENT_3D ( 'NONE', #13848, #7543, #12613 ) ;
#7665 = LINE ( 'NONE', #15463, #15580 ) ;
#7666 = CARTESIAN_POINT ( 'NONE',  ( 49.86468353125000164, 26.85937500034139802, -6.106662507704105588E-15 ) ) ;
#7667 = ORIENTED_EDGE ( 'NONE', *, *, #7031, .T. ) ;
#7668 = CARTESIAN_POINT ( 'NONE',  ( 49.99999999999999289, 33.10000000000000142, -16.24598481164532160 ) ) ;
#7669 = CYLINDRICAL_SURFACE ( 'NONE', #943, 50.00000000000000000 ) ;
#7670 = CARTESIAN_POINT ( 'NONE',  ( 45.11452830843730766, 25.00000000000000355, -21.24066852005663719 ) ) ;
#7671 = CARTESIAN_POINT ( 'NONE',  ( 9.631387414534489405E-15, 36.42187500034139447, 52.43083105670540789 ) ) ;
#7672 = CARTESIAN_POINT ( 'NONE',  ( -2.445080149700054274E-14, 46.28125000068280315, 50.00000000000000000 ) ) ;
#7673 = CARTESIAN_POINT ( 'NONE',  ( -49.86468353124999453, 25.95937500034139589, 16.20201782572377169 ) ) ;
#7674 = CARTESIAN_POINT ( 'NONE',  ( 0.000000000000000000, 25.00000000000000000, -50.00000000000000000 ) ) ;
#7675 = CARTESIAN_POINT ( 'NONE',  ( -30.81806926056963292, 35.62187500034140442, -42.41743335407646498 ) ) ;
#7676 = CARTESIAN_POINT ( 'NONE',  ( -15.45084971874736368, 30.18125000068280173, 47.55282581475768211 ) ) ;
#7677 = AXIS2_PLACEMENT_3D ( 'NONE', #8051, #6905, #7893 ) ;
#7678 = CARTESIAN_POINT ( 'NONE',  ( 40.45084971874737079, 31.20000000000000284, -29.38926261462366440 ) ) ;
#7679 = CARTESIAN_POINT ( 'NONE',  ( -3.210462471511496205E-15, 37.35937500034139447, -52.43083105670540789 ) ) ;
#7680 = CARTESIAN_POINT ( 'NONE',  ( 15.40903463028482356, 32.52187500034139589, 47.42413220539093999 ) ) ;
#7681 = CARTESIAN_POINT ( 'NONE',  ( 30.90169943749474157, 43.30000000000000426, -42.53254041760200721 ) ) ;
#7682 = EDGE_CURVE ( 'NONE', #2064, #6657, #13684, .T. ) ;
#7683 = ORIENTED_EDGE ( 'NONE', *, *, #14127, .F. ) ;
#7684 = VERTEX_POINT ( 'NONE', #11698 ) ;
#7685 = CARTESIAN_POINT ( 'NONE',  ( -49.86468353125000164, 37.85937500034139447, 0.000000000000000000 ) ) ;
#7686 = ORIENTED_EDGE ( 'NONE', *, *, #13835, .T. ) ;
#7687 = ORIENTED_EDGE ( 'NONE', *, *, #10887, .T. ) ;
#7688 = CARTESIAN_POINT ( 'NONE',  ( 26.69586624684728093, 283.2330659412872933, -5.891732493678564886 ) ) ;
#7689 = CARTESIAN_POINT ( 'NONE',  ( 49.86468353124999453, 48.95937500034140299, -16.20201782572376459 ) ) ;
#7690 = CARTESIAN_POINT ( 'NONE',  ( 0.000000000000000000, 267.0000000000000000, 0.000000000000000000 ) ) ;
#7691 = CARTESIAN_POINT ( 'NONE',  ( -15.40903463028481646, 21.52187500034139589, -47.42413220539093999 ) ) ;
#7692 = DIRECTION ( 'NONE',  ( 0.000000000000000000, -1.541976423090494894E-16, -1.000000000000000000 ) ) ;
#7693 = CARTESIAN_POINT ( 'NONE',  ( 40.34137639590981905, 44.72187500034139163, 29.30972558990010768 ) ) ;
#7694 = CARTESIAN_POINT ( 'NONE',  ( 49.86468353124999453, 40.95937500034140299, -16.20201782572376104 ) ) ;
#7695 = DIRECTION ( 'NONE',  ( 0.9510565162951544194, -0.3090169943749448422, 0.000000000000000000 ) ) ;
#7696 = CARTESIAN_POINT ( 'NONE',  ( 15.45084971874737789, 48.60000000000000142, 47.55282581475767500 ) ) ;
#7697 = CARTESIAN_POINT ( 'NONE',  ( 15.45084971874737789, 26.38125000068280102, 47.55282581475767500 ) ) ;
#7698 = CARTESIAN_POINT ( 'NONE',  ( 10.22617902976740822, 36.71297534007683794, 92.96698611470405638 ) ) ;
#7699 = CONICAL_SURFACE ( 'NONE', #6380, 85.01963570546854498, 0.9599310885968793672 ) ;
#7700 = CARTESIAN_POINT ( 'NONE',  ( 30.81806926056964002, 34.62187500034139731, 42.41743335407647209 ) ) ;
#7701 = DIRECTION ( 'NONE',  ( -6.938893903907231459E-18, 1.000000000000000000, 5.551115123125782702E-17 ) ) ;
#7702 = ORIENTED_EDGE ( 'NONE', *, *, #3975, .F. ) ;
#7703 = ORIENTED_EDGE ( 'NONE', *, *, #4905, .T. ) ;
#7704 = CARTESIAN_POINT ( 'NONE',  ( 19.99999999999999645, 307.0000000000000568, -2.499999999999999556 ) ) ;
#7705 = DIRECTION ( 'NONE',  ( 0.000000000000000000, 0.000000000000000000, 1.000000000000000000 ) ) ;
#7706 = DIRECTION ( 'NONE',  ( 0.000000000000000000, 0.000000000000000000, 1.000000000000000000 ) ) ;
#7707 = CARTESIAN_POINT ( 'NONE',  ( -30.90169943749474513, 23.48125000068279888, -42.53254041760200721 ) ) ;
#7708 = EDGE_CURVE ( 'NONE', #15481, #15953, #2473, .T. ) ;
#7709 = CARTESIAN_POINT ( 'NONE',  ( -15.40903463028480580, 34.25937500034139305, 47.42413220539094709 ) ) ;
#7710 = DIRECTION ( 'NONE',  ( -6.938893903907231459E-18, 1.000000000000000000, 5.551115123125782702E-17 ) ) ;
#7711 = CARTESIAN_POINT ( 'NONE',  ( 49.86468353125000164, 48.92187500034139447, -6.106662507704105588E-15 ) ) ;
#7712 = DIRECTION ( 'NONE',  ( 0.000000000000000000, -0.5735764363510476027, -0.8191520442889907994 ) ) ;
#7713 = CARTESIAN_POINT ( 'NONE',  ( -15.45084971874737256, 35.38125000068279746, -47.55282581475767500 ) ) ;
#7714 = DIRECTION ( 'NONE',  ( 0.000000000000000000, -0.000000000000000000, 1.000000000000000000 ) ) ;
#7715 = ORIENTED_EDGE ( 'NONE', *, *, #7682, .F. ) ;
#7716 = CARTESIAN_POINT ( 'NONE',  ( 15.40903463028482356, 20.45937500034139589, 47.42413220539093999 ) ) ;
#7717 = PRODUCT ( 'Heavy Glass Blender Jar Body', 'Heavy Glass Blender Jar Body', '', ( #15605 ) ) ;
#7718 = ORIENTED_EDGE ( 'NONE', *, *, #11659, .T. ) ;
#7719 = CARTESIAN_POINT ( 'NONE',  ( -3.111920190527341144E-15, 27.28125000068279604, -50.00000000000000000 ) ) ;
#7720 = ADVANCED_FACE ( 'NONE', ( #1631 ), #12952, .T. ) ;
#7721 = ORIENTED_EDGE ( 'NONE', *, *, #2441, .F. ) ;
#7722 = ORIENTED_EDGE ( 'NONE', *, *, #6936, .T. ) ;
#7723 = DIRECTION ( 'NONE',  ( -0.000000000000000000, -1.000000000000000000, -0.000000000000000000 ) ) ;
#7724 = CARTESIAN_POINT ( 'NONE',  ( 7.164845293663816506, 37.36320934111687109, 102.0000000000000142 ) ) ;
#7725 = CARTESIAN_POINT ( 'NONE',  ( -5.000000000000000000, 96.75198296766782846, -7.580410092413988998 ) ) ;
#7726 = DIRECTION ( 'NONE',  ( 1.000000000000000000, 0.000000000000000000, 0.000000000000000000 ) ) ;
#7727 = CARTESIAN_POINT ( 'NONE',  ( -16.34981105473763563, 20.27881147257167527, 102.0000000000000142 ) ) ;
#7728 = CYLINDRICAL_SURFACE ( 'NONE', #15568, 50.00000000000000000 ) ;
#7729 = PLANE ( 'NONE',  #1679 ) ;
#7730 = CARTESIAN_POINT ( 'NONE',  ( 5.988468393966018155, 15.10823117958429584, 102.0000000000000142 ) ) ;
#7731 = SURFACE_STYLE_FILL_AREA ( #11471 ) ;
#7732 = CARTESIAN_POINT ( 'NONE',  ( 10.68655108903834794, 8.641875097208380652, 101.0000000000000000 ) ) ;
#7733 = CARTESIAN_POINT ( 'NONE',  ( 50.00000000000000000, 38.78125000068279604, -6.123233995736766085E-15 ) ) ;
#7734 = CARTESIAN_POINT ( 'NONE',  ( -33.58330087751641457, 35.02991267065630154, 22.31061932476987053 ) ) ;
#7735 = EDGE_CURVE ( 'NONE', #14050, #1840, #1960, .T. ) ;
#7736 = CARTESIAN_POINT ( 'NONE',  ( 40.45084971874737789, 22.80000000000000071, 29.38926261462365375 ) ) ;
#7737 = SURFACE_SIDE_STYLE ('',( #15293 ) ) ;
#7738 = ORIENTED_EDGE ( 'NONE', *, *, #13650, .F. ) ;
#7739 = CARTESIAN_POINT ( 'NONE',  ( -15.40903463028481646, 39.45937500034139589, -47.42413220539093999 ) ) ;
#7740 = VERTEX_POINT ( 'NONE', #14993 ) ;
#7741 = CARTESIAN_POINT ( 'NONE',  ( -3.111920190527341144E-15, 43.28125000068280315, -50.00000000000000000 ) ) ;
#7742 = DIRECTION ( 'NONE',  ( 0.000000000000000000, 0.000000000000000000, 1.000000000000000000 ) ) ;
#7743 = CARTESIAN_POINT ( 'NONE',  ( 15.40903463028482356, 28.45937500034139589, 47.42413220539093999 ) ) ;
#7744 = VERTEX_POINT ( 'NONE', #11435 ) ;
#7745 = EDGE_CURVE ( 'NONE', #9153, #9017, #8767, .T. ) ;
#7746 = CARTESIAN_POINT ( 'NONE',  ( 40.45084971874737079, 33.20000000000000284, -29.38926261462366440 ) ) ;
#7747 = CARTESIAN_POINT ( 'NONE',  ( -16.62039348561838281, 28.09550434916130257, 93.58242969371653430 ) ) ;
#7748 = CARTESIAN_POINT ( 'NONE',  ( 47.07787634996847714, 25.00000000000000000, -16.43739640347052955 ) ) ;
#7749 = CARTESIAN_POINT ( 'NONE',  ( -40.34137639590981905, 31.72187500034139873, -29.30972558990011478 ) ) ;
#7750 = CARTESIAN_POINT ( 'NONE',  ( 0.000000000000000000, 193.4213562373095385, 0.000000000000000000 ) ) ;
#7751 = CARTESIAN_POINT ( 'NONE',  ( 49.86468353125000164, 22.85937500034139802, -6.106662507704105588E-15 ) ) ;
#7752 = DIRECTION ( 'NONE',  ( 0.000000000000000000, 0.000000000000000000, -1.000000000000000000 ) ) ;
#7753 = CARTESIAN_POINT ( 'NONE',  ( -15.40903463028481646, 31.52187500034139944, -47.42413220539093999 ) ) ;
#7754 = CARTESIAN_POINT ( 'NONE',  ( -7.499999999999994671, 40.00000000000000711, -24.29058411375428150 ) ) ;
#7755 = CARTESIAN_POINT ( 'NONE',  ( -30.90169943749474868, 29.70000000000000284, -42.53254041760200721 ) ) ;
#7756 = CARTESIAN_POINT ( 'NONE',  ( -30.81806926056962226, 34.15937500034139163, 42.41743335407647919 ) ) ;
#7757 = CARTESIAN_POINT ( 'NONE',  ( -3.210462471511496205E-15, 33.42187500034140157, -52.43083105670540789 ) ) ;
#7758 = CARTESIAN_POINT ( 'NONE',  ( 15.45084971874736723, 41.40000000000000568, -47.55282581475768211 ) ) ;
#7759 = VERTEX_POINT ( 'NONE', #7519 ) ;
#7760 = UNCERTAINTY_MEASURE_WITH_UNIT (LENGTH_MEASURE( 1.000000000000000082E-05 ), #3062, 'distance_accuracy_value', 'NONE');
#7761 = CARTESIAN_POINT ( 'NONE',  ( -49.86468353124999453, 37.95937500034139589, 16.20201782572377169 ) ) ;
#7762 = VERTEX_POINT ( 'NONE', #8686 ) ;
#7763 = ADVANCED_FACE ( 'NONE', ( #5133 ), #9939, .F. ) ;
#7764 = CARTESIAN_POINT ( 'NONE',  ( 20.31983351293479956, 285.7035871579556670, -7.659916756470847687 ) ) ;
#7765 = CARTESIAN_POINT ( 'NONE',  ( 49.86468353125000164, 46.85937500034139447, -6.106662507704105588E-15 ) ) ;
#7766 = EDGE_CURVE ( 'NONE', #5908, #1328, #10029, .T. ) ;
#7767 = FACE_OUTER_BOUND ( 'NONE', #21, .T. ) ;
#7768 = CARTESIAN_POINT ( 'NONE',  ( -49.86468353124999453, 26.02187500034139944, 16.20201782572377525 ) ) ;
#7769 = CARTESIAN_POINT ( 'NONE',  ( -3.407225380398804404, 31.38205016914259105, 101.0000000000000000 ) ) ;
#7770 = CARTESIAN_POINT ( 'NONE',  ( 49.86468353125000164, 34.92187500034140157, -6.106662507704105588E-15 ) ) ;
#7771 = CARTESIAN_POINT ( 'NONE',  ( -40.34137639590981195, 40.05937500034140442, 29.30972558990012189 ) ) ;
#7772 = CARTESIAN_POINT ( 'NONE',  ( 0.000000000000000000, 257.0000000000001137, 45.00000000000000000 ) ) ;
#7773 = CARTESIAN_POINT ( 'NONE',  ( 30.90169943749474157, 45.29999999999999005, -42.53254041760200721 ) ) ;
#7774 = VECTOR ( 'NONE', #14270, 999.9999999999998863 ) ;
#7775 = CARTESIAN_POINT ( 'NONE',  ( 15.45084971874736723, 25.18125000068279817, -47.55282581475768211 ) ) ;
#7776 = CARTESIAN_POINT ( 'NONE',  ( 12.80943516814229532, 34.43714179323908553, 93.05110628388169403 ) ) ;
#7777 = CARTESIAN_POINT ( 'NONE',  ( 49.86468353125001585, 28.82187500034139305, 16.20201782572375038 ) ) ;
#7778 = EDGE_CURVE ( 'NONE', #871, #13942, #1105, .T. ) ;
#7779 = CARTESIAN_POINT ( 'NONE',  ( 0.000000000000000000, 272.0000000000000000, 0.000000000000000000 ) ) ;
#7780 = ADVANCED_FACE ( 'NONE', ( #8936 ), #10269, .F. ) ;
#7781 = VERTEX_POINT ( 'NONE', #11273 ) ;
#7782 = CARTESIAN_POINT ( 'NONE',  ( 30.90169943749474157, 37.08125000068279320, -42.53254041760200721 ) ) ;
#7783 = VECTOR ( 'NONE', #10944, 1000.000000000000000 ) ;
#7784 = VERTEX_POINT ( 'NONE', #12683 ) ;
#7785 = LINE ( 'NONE', #1705, #12939 ) ;
#7786 = DIRECTION ( 'NONE',  ( 0.8090169943749426773, 0.5877852522924797984, 0.000000000000000000 ) ) ;
#7787 = ADVANCED_FACE ( 'NONE', ( #2614 ), #4968, .T. ) ;
#7788 = FACE_OUTER_BOUND ( 'NONE', #7261, .T. ) ;
#7789 = CARTESIAN_POINT ( 'NONE',  ( 15.40903463028482356, 48.52187500034140299, 47.42413220539093999 ) ) ;
#7790 = CARTESIAN_POINT ( 'NONE',  ( -40.34137639590981905, 31.65937500034139873, -29.30972558990011478 ) ) ;
#7791 = CARTESIAN_POINT ( 'NONE',  ( -49.86468353125000164, 43.92187500034140157, 0.000000000000000000 ) ) ;
#7792 = DIRECTION ( 'NONE',  ( 0.000000000000000000, 0.000000000000000000, 1.000000000000000000 ) ) ;
#7793 = FACE_OUTER_BOUND ( 'NONE', #9222, .T. ) ;
#7794 = AXIS2_PLACEMENT_3D ( 'NONE', #6000, #7084, #11070 ) ;
#7795 = CARTESIAN_POINT ( 'NONE',  ( 5.143516556418884111E-15, 54.99999999999999289, 42.00000000000000711 ) ) ;
#7796 = CARTESIAN_POINT ( 'NONE',  ( 30.90169943749475223, 28.48125000068279888, 42.53254041760199300 ) ) ;
#7797 = VERTEX_POINT ( 'NONE', #12592 ) ;
#7798 = CARTESIAN_POINT ( 'NONE',  ( -15.40903463028480580, 20.25937500034139660, 47.42413220539094709 ) ) ;
#7799 = ORIENTED_EDGE ( 'NONE', *, *, #1880, .T. ) ;
#7800 = DIRECTION ( 'NONE',  ( -1.000000000000000000, 0.000000000000000000, -0.000000000000000000 ) ) ;
#7801 = ORIENTED_EDGE ( 'NONE', *, *, #13221, .T. ) ;
#7802 = EDGE_LOOP ( 'NONE', ( #15975, #14946, #13498, #11708 ) ) ;
#7803 = CARTESIAN_POINT ( 'NONE',  ( 9.262651381018932677E-15, 102.0000000000000142, -9.080892972013931086 ) ) ;
#7804 = DIRECTION ( 'NONE',  ( 1.000000000000000000, 0.000000000000000000, 0.000000000000000000 ) ) ;
#7805 = VECTOR ( 'NONE', #14366, 1000.000000000000000 ) ;
#7806 = CARTESIAN_POINT ( 'NONE',  ( -30.90169943749473802, 22.30000000000000071, 42.53254041760200721 ) ) ;
#7807 = DIRECTION ( 'NONE',  ( 1.000000000000000000, 0.000000000000000000, 0.000000000000000000 ) ) ;
#7808 = DIRECTION ( 'NONE',  ( -0.000000000000000000, 0.000000000000000000, 1.000000000000000000 ) ) ;
#7809 = CARTESIAN_POINT ( 'NONE',  ( -30.90169943749474513, 31.48125000068279533, -42.53254041760200721 ) ) ;
#7810 = CARTESIAN_POINT ( 'NONE',  ( 15.45084971874737789, 24.38125000068279746, 47.55282581475767500 ) ) ;
#7811 = CARTESIAN_POINT ( 'NONE',  ( 15.40903463028481113, 25.32187500034139660, -47.42413220539094709 ) ) ;
#7812 = DIRECTION ( 'NONE',  ( 0.000000000000000000, -1.000000000000000000, 0.000000000000000000 ) ) ;
#7813 = CARTESIAN_POINT ( 'NONE',  ( -40.45084971874737079, 37.98125000068279888, 29.38926261462367151 ) ) ;
#7814 = CARTESIAN_POINT ( 'NONE',  ( 0.000000000000000000, 272.0000000000000000, 79.49773270518484480 ) ) ;
#7815 = CARTESIAN_POINT ( 'NONE',  ( 4.320770838041294581, 30.97531352606685218, 102.0000000000000142 ) ) ;
#7816 = ORIENTED_EDGE ( 'NONE', *, *, #9009, .T. ) ;
#7817 = CIRCLE ( 'NONE', #629, 17.50000000000000000 ) ;
#7818 = CARTESIAN_POINT ( 'NONE',  ( 40.34137639590981195, 39.05937500034140442, -29.30972558990011834 ) ) ;
#7819 = ORIENTED_EDGE ( 'NONE', *, *, #13921, .F. ) ;
#7820 = SURFACE_STYLE_FILL_AREA ( #10081 ) ;
#7821 = PLANE ( 'NONE',  #442 ) ;
#7822 = CARTESIAN_POINT ( 'NONE',  ( 15.40903463028481113, 31.25937500034140015, -47.42413220539094709 ) ) ;
#7823 = ADVANCED_FACE ( 'NONE', ( #11508, #7767 ), #12837, .T. ) ;
#7824 = ORIENTED_EDGE ( 'NONE', *, *, #13293, .T. ) ;
#7825 = CARTESIAN_POINT ( 'NONE',  ( 6.123233995736766085E-15, 193.4213562373095385, 50.00000000000000000 ) ) ;
#7826 = CARTESIAN_POINT ( 'NONE',  ( -6.000000000000001776, 22.50000000000000000, 101.0000000000000000 ) ) ;
#7827 = CONICAL_SURFACE ( 'NONE', #10495, 16.50000000000000711, 0.7853981633974447263 ) ;
#7828 = LINE ( 'NONE', #12903, #2469 ) ;
#7829 = CARTESIAN_POINT ( 'NONE',  ( 49.86468353125000164, 34.92187500034140157, -6.106662507704105588E-15 ) ) ;
#7830 = DIRECTION ( 'NONE',  ( 0.000000000000000000, -0.000000000000000000, 1.000000000000000000 ) ) ;
#7831 = CARTESIAN_POINT ( 'NONE',  ( -30.81806926056963292, 25.55937500034139376, -42.41743335407646498 ) ) ;
#7832 = CARTESIAN_POINT ( 'NONE',  ( 30.90169943749475223, 42.69999999999999574, 42.53254041760199300 ) ) ;
#7833 = CARTESIAN_POINT ( 'NONE',  ( -3.210462471511496205E-15, 31.42187500034139447, -52.43083105670540789 ) ) ;
#7834 = EDGE_CURVE ( 'NONE', #384, #6400, #6449, .T. ) ;
#7835 = CARTESIAN_POINT ( 'NONE',  ( -49.99999999999999289, 22.09999999999999787, 16.24598481164533226 ) ) ;
#7836 = EDGE_CURVE ( 'NONE', #4422, #4896, #9666, .T. ) ;
#7837 = CARTESIAN_POINT ( 'NONE',  ( 30.90169943749475578, 32.70000000000000284, 42.53254041760200010 ) ) ;
#7838 = CARTESIAN_POINT ( 'NONE',  ( 9.631387414534489405E-15, 30.35937500034139447, 52.43083105670540789 ) ) ;
#7839 = CARTESIAN_POINT ( 'NONE',  ( -40.34137639590981905, 29.72187500034139518, -29.30972558990011478 ) ) ;
#7840 = ADVANCED_FACE ( 'NONE', ( #8849, #13909 ), #2528, .F. ) ;
#7841 = ORIENTED_EDGE ( 'NONE', *, *, #11329, .F. ) ;
#7842 = AXIS2_PLACEMENT_3D ( 'NONE', #965, #13602, #2053 ) ;
#7843 = CARTESIAN_POINT ( 'NONE',  ( -15.40903463028481646, 37.45937500034139589, -47.42413220539093999 ) ) ;
#7844 = ORIENTED_EDGE ( 'NONE', *, *, #7330, .T. ) ;
#7845 = CARTESIAN_POINT ( 'NONE',  ( 25.15991675647082815, 285.7035871579557806, -2.819833512935952413 ) ) ;
#7846 = CARTESIAN_POINT ( 'NONE',  ( 49.86468353125001585, 46.75937500034140015, 16.20201782572375038 ) ) ;
#7847 = CARTESIAN_POINT ( 'NONE',  ( -25.00000000000000355, 307.0000000000000568, 7.500000000000001776 ) ) ;
#7848 = CARTESIAN_POINT ( 'NONE',  ( -40.34137639590981195, 26.12187500034139731, 29.30972558990012189 ) ) ;
#7849 = CARTESIAN_POINT ( 'NONE',  ( -25.48725218878006160, 284.2907069533295612, 7.987252188781084783 ) ) ;
#7850 = CARTESIAN_POINT ( 'NONE',  ( 9.631387414534489405E-15, 34.42187500034138736, 52.43083105670540789 ) ) ;
#7851 = CARTESIAN_POINT ( 'NONE',  ( 40.34137639590981905, 44.65937500034139163, 29.30972558990010768 ) ) ;
#7852 = CIRCLE ( 'NONE', #12894, 17.50000000000000000 ) ;
#7853 = CARTESIAN_POINT ( 'NONE',  ( -40.45084971874737789, 25.58125000068279675, -29.38926261462365730 ) ) ;
#7854 = VECTOR ( 'NONE', #1460, 999.9999999999998863 ) ;
#7855 = CARTESIAN_POINT ( 'NONE',  ( -49.86468353125000164, 19.92187500034139447, 0.000000000000000000 ) ) ;
#7856 = CARTESIAN_POINT ( 'NONE',  ( -30.90169943749473802, 22.08125000068279320, 42.53254041760200721 ) ) ;
#7857 = CARTESIAN_POINT ( 'NONE',  ( 15.40903463028481113, 49.32187500034139305, -47.42413220539094709 ) ) ;
#7858 = CARTESIAN_POINT ( 'NONE',  ( -30.81806926056962226, 28.22187500034139873, 42.41743335407647919 ) ) ;
#7859 = LINE ( 'NONE', #6461, #10209 ) ;
#7860 = ORIENTED_EDGE ( 'NONE', *, *, #16301, .F. ) ;
#7861 = VECTOR ( 'NONE', #576, 1000.000000000000000 ) ;
#7862 = VECTOR ( 'NONE', #5558, 1000.000000000000000 ) ;
#7864 = CARTESIAN_POINT ( 'NONE',  ( 49.99999999999999289, 34.88125000068279746, -16.24598481164532160 ) ) ;
#7863 = VECTOR ( 'NONE', #8780, 1000.000000000000000 ) ;
#7865 = EDGE_LOOP ( 'NONE', ( #4525, #11866, #7475, #14355 ) ) ;
#7866 = CARTESIAN_POINT ( 'NONE',  ( 40.45084971874737789, 48.58125000068280031, 29.38926261462365375 ) ) ;
#7867 = DIRECTION ( 'NONE',  ( 0.000000000000000000, 0.000000000000000000, -1.000000000000000000 ) ) ;
#7868 = DIRECTION ( 'NONE',  ( 0.000000000000000000, 0.000000000000000000, -1.000000000000000000 ) ) ;
#7869 = CARTESIAN_POINT ( 'NONE',  ( 15.40903463028481113, 47.32187500034140015, -47.42413220539094709 ) ) ;
#7870 = CARTESIAN_POINT ( 'NONE',  ( 40.34137639590981905, 22.65937500034139518, 29.30972558990010768 ) ) ;
#7871 = CARTESIAN_POINT ( 'NONE',  ( 37.77664397204034685, 25.00000000000000355, -13.15010152849429481 ) ) ;
#7872 = CARTESIAN_POINT ( 'NONE',  ( -30.81806926056963292, 45.62187500034139020, -42.41743335407646498 ) ) ;
#7873 = AXIS2_PLACEMENT_3D ( 'NONE', #9929, #7189, #14983 ) ;
#7875 = CARTESIAN_POINT ( 'NONE',  ( 1.671572875253809487, 246.1715728752537871, -50.00000000000000000 ) ) ;
#7874 = AXIS2_PLACEMENT_3D ( 'NONE', #8488, #1758, #3676 ) ;
#7876 = CARTESIAN_POINT ( 'NONE',  ( -3.210462471511496205E-15, 45.42187500034139447, -52.43083105670540789 ) ) ;
#7877 = CARTESIAN_POINT ( 'NONE',  ( 40.45084971874737079, 28.98125000068279888, -29.38926261462366440 ) ) ;
#7878 = ORIENTED_EDGE ( 'NONE', *, *, #14773, .F. ) ;
#7879 = CARTESIAN_POINT ( 'NONE',  ( -30.81806926056962226, 48.22187500034139163, 42.41743335407647919 ) ) ;
#7880 = EDGE_CURVE ( 'NONE', #11917, #3234, #15240, .T. ) ;
#7881 = VERTEX_POINT ( 'NONE', #12142 ) ;
#7882 = CARTESIAN_POINT ( 'NONE',  ( 0.000000000000000000, 0.000000000000000000, -5.000000000000000000 ) ) ;
#7883 = ORIENTED_EDGE ( 'NONE', *, *, #6418, .T. ) ;
#7884 = VERTEX_POINT ( 'NONE', #272 ) ;
#7885 = AXIS2_PLACEMENT_3D ( 'NONE', #14604, #12285, #14527 ) ;
#7886 = CARTESIAN_POINT ( 'NONE',  ( 0.000000000000000000, 52.00000000000000711, 0.000000000000000000 ) ) ;
#7887 = CARTESIAN_POINT ( 'NONE',  ( 0.000000000000000000, 20.00000000000000355, 0.000000000000000000 ) ) ;
#7888 = VECTOR ( 'NONE', #10559, 1000.000000000000000 ) ;
#7889 = CARTESIAN_POINT ( 'NONE',  ( -9.151574469205250750, 1.945227203041358877, 101.0000000000000000 ) ) ;
#7890 = CARTESIAN_POINT ( 'NONE',  ( 40.45084971874737789, 24.80000000000000426, 29.38926261462365375 ) ) ;
#7891 = CARTESIAN_POINT ( 'NONE',  ( 40.34137639590981905, 46.65937500034139873, 29.30972558990010768 ) ) ;
#7892 = CARTESIAN_POINT ( 'NONE',  ( 15.45084971874736723, 49.18125000068279462, -47.55282581475768211 ) ) ;
#7893 = DIRECTION ( 'NONE',  ( -1.000000000000000000, 0.000000000000000000, 0.000000000000000000 ) ) ;
#7894 = CARTESIAN_POINT ( 'NONE',  ( 15.40903463028481113, 21.32187500034139660, -47.42413220539094709 ) ) ;
#7895 = FILL_AREA_STYLE_COLOUR ( '', #12889 ) ;
#7896 = DIRECTION ( 'NONE',  ( -0.6691306063588567943, -0.7431448254773955764, 0.000000000000000000 ) ) ;
#7897 = CARTESIAN_POINT ( 'NONE',  ( 50.00000000000000000, 40.78125000068279604, -6.123233995736766085E-15 ) ) ;
#7898 = CARTESIAN_POINT ( 'NONE',  ( -40.45084971874737079, 37.98125000068279888, 29.38926261462367151 ) ) ;
#7899 = CARTESIAN_POINT ( 'NONE',  ( 50.00000000000000000, 22.78125000068279959, -6.123233995736766085E-15 ) ) ;
#7900 = DIRECTION ( 'NONE',  ( 0.000000000000000000, 0.000000000000000000, -1.000000000000000000 ) ) ;
#7901 = ORIENTED_EDGE ( 'NONE', *, *, #5909, .T. ) ;
#7902 = CARTESIAN_POINT ( 'NONE',  ( -49.86468353125000164, 35.85937500034140157, 0.000000000000000000 ) ) ;
#7903 = ORIENTED_EDGE ( 'NONE', *, *, #14133, .F. ) ;
#7904 = CARTESIAN_POINT ( 'NONE',  ( 40.45084971874737789, 48.58125000068280031, 29.38926261462365375 ) ) ;
#7905 = CARTESIAN_POINT ( 'NONE',  ( 24.99999999999999645, 307.0000000000000568, 7.500000000000002665 ) ) ;
#7906 = CARTESIAN_POINT ( 'NONE',  ( 15.40903463028481113, 23.25937500034139660, -47.42413220539094709 ) ) ;
#7907 = VERTEX_POINT ( 'NONE', #13005 ) ;
#7908 = LINE ( 'NONE', #10163, #13692 ) ;
#7909 = CARTESIAN_POINT ( 'NONE',  ( -12.00394982932901655, 35.24696676550272656, 93.01447361572049033 ) ) ;
#7910 = CARTESIAN_POINT ( 'NONE',  ( 7.574663982647604321, 38.28367718720770796, 101.0000000000000000 ) ) ;
#7911 = CARTESIAN_POINT ( 'NONE',  ( -40.34137639590981195, 26.12187500034139731, 29.30972558990012189 ) ) ;
#7912 = EDGE_CURVE ( 'NONE', #15952, #2027, #10738, .T. ) ;
#7913 = CARTESIAN_POINT ( 'NONE',  ( -7.574663982647817484, 38.28367718720760138, 101.0000000000000000 ) ) ;
#7914 = EDGE_CURVE ( 'NONE', #10580, #3182, #4371, .T. ) ;
#7915 = CARTESIAN_POINT ( 'NONE',  ( 7.919222016226827421, 47.44874571845315359, -50.00000000000000000 ) ) ;
#7916 = CARTESIAN_POINT ( 'NONE',  ( -48.34710198928235059, 20.00000000000000355, 12.20844498793695365 ) ) ;
#7917 = CARTESIAN_POINT ( 'NONE',  ( 30.81806926056964002, 30.62187500034139376, 42.41743335407646498 ) ) ;
#7918 = CARTESIAN_POINT ( 'NONE',  ( -5.000000000000000000, 99.58041009241402719, -7.580410092413988998 ) ) ;
#7919 = CARTESIAN_POINT ( 'NONE',  ( -40.45084971874737789, 29.80000000000000071, -29.38926261462365730 ) ) ;
#7920 = CARTESIAN_POINT ( 'NONE',  ( -49.86468353124999453, 33.95937500034139589, 16.20201782572377525 ) ) ;
#7921 = CARTESIAN_POINT ( 'NONE',  ( -40.34137639590981905, 27.72187500034139873, -29.30972558990011478 ) ) ;
#7922 = CARTESIAN_POINT ( 'NONE',  ( 50.00000000000000000, 39.00000000000000000, -6.123233995736766085E-15 ) ) ;
#7923 = AXIS2_PLACEMENT_3D ( 'NONE', #10206, #11214, #10046 ) ;
#7924 = VERTEX_POINT ( 'NONE', #14244 ) ;
#7925 = PRODUCT_DEFINITION_CONTEXT ( 'detailed design', #6668, 'design' ) ;
#7926 = CARTESIAN_POINT ( 'NONE',  ( 15.40903463028481113, 27.25937500034139660, -47.42413220539094709 ) ) ;
#7927 = ORIENTED_EDGE ( 'NONE', *, *, #701, .T. ) ;
#7928 = ADVANCED_FACE ( 'NONE', ( #14698 ), #2863, .F. ) ;
#7929 = CARTESIAN_POINT ( 'NONE',  ( 25.56848793686463139, 282.5058351977235134, -10.28424396843206523 ) ) ;
#7930 = CARTESIAN_POINT ( 'NONE',  ( 30.81806926056964002, 48.55937500034138310, 42.41743335407647209 ) ) ;
#7931 = DIRECTION ( 'NONE',  ( 1.000000000000000000, 0.000000000000000000, 0.000000000000000000 ) ) ;
#7932 = CARTESIAN_POINT ( 'NONE',  ( 25.07567824489208164, 285.0109613521088932, 7.575678244891727253 ) ) ;
#7933 = CARTESIAN_POINT ( 'NONE',  ( -29.01527194596179271, 282.0655843567852799, 11.51527194596495463 ) ) ;
#7934 = AXIS2_PLACEMENT_3D ( 'NONE', #5172, #3829, #10229 ) ;
#7935 = CARTESIAN_POINT ( 'NONE',  ( -3.210462471511496205E-15, 33.42187500034140157, -52.43083105670540789 ) ) ;
#7936 = CARTESIAN_POINT ( 'NONE',  ( 49.86468353125000164, 38.85937500034139447, -6.106662507704105588E-15 ) ) ;
#7937 = CARTESIAN_POINT ( 'NONE',  ( -9.485510086921518536, 8.593664601562084115, 101.6666710451724214 ) ) ;
#7938 = CARTESIAN_POINT ( 'NONE',  ( -15.45084971874736368, 38.40000000000000568, 47.55282581475768211 ) ) ;
#7939 = CARTESIAN_POINT ( 'NONE',  ( 15.40903463028481113, 49.25937500034139305, -47.42413220539094709 ) ) ;
#7940 = CARTESIAN_POINT ( 'NONE',  ( -3.210462471511496205E-15, 47.42187500034138736, -52.43083105670540789 ) ) ;
#7941 = EDGE_CURVE ( 'NONE', #16202, #14151, #11802, .T. ) ;
#7942 = CARTESIAN_POINT ( 'NONE',  ( -30.81806926056962226, 26.22187500034139518, 42.41743335407647919 ) ) ;
#7943 = VECTOR ( 'NONE', #10128, 1000.000000000000000 ) ;
#7944 = CARTESIAN_POINT ( 'NONE',  ( -50.00000000000000000, 27.78125000068279959, 0.000000000000000000 ) ) ;
#7945 = ORIENTED_EDGE ( 'NONE', *, *, #16408, .T. ) ;
#7946 = CARTESIAN_POINT ( 'NONE',  ( 15.45084971874737789, 34.38125000068280457, 47.55282581475767500 ) ) ;
#7947 = EDGE_CURVE ( 'NONE', #11302, #10383, #3325, .T. ) ;
#7948 = EDGE_LOOP ( 'NONE', ( #2956, #8879 ) ) ;
#7949 = CARTESIAN_POINT ( 'NONE',  ( 7.919222016226818539, 49.22999571913594252, -50.00000000000000000 ) ) ;
#7950 = CARTESIAN_POINT ( 'NONE',  ( 2.500000000000000000, 242.0000000000000284, 40.00000000000000000 ) ) ;
#7951 = EDGE_CURVE ( 'NONE', #2544, #12958, #7817, .T. ) ;
#7952 = CARTESIAN_POINT ( 'NONE',  ( 15.45084971874736723, 33.18125000068279462, -47.55282581475768211 ) ) ;
#7953 = CARTESIAN_POINT ( 'NONE',  ( 30.81806926056962936, 45.22187500034139873, -42.41743335407646498 ) ) ;
#7954 = CARTESIAN_POINT ( 'NONE',  ( 30.81806926056962936, 23.15937500034139873, -42.41743335407647209 ) ) ;
#7955 = CARTESIAN_POINT ( 'NONE',  ( -40.45084971874737079, 39.98125000068279888, 29.38926261462367151 ) ) ;
#7956 = CARTESIAN_POINT ( 'NONE',  ( 49.86468353125000164, 42.92187500034140157, -6.106662507704105588E-15 ) ) ;
#7957 = AXIS2_PLACEMENT_3D ( 'NONE', #12549, #12717, #15367 ) ;
#7958 = CARTESIAN_POINT ( 'NONE',  ( -2.547328955960238000E-13, 34.28125000068279604, 49.99999999999999289 ) ) ;
#7959 = CARTESIAN_POINT ( 'NONE',  ( 15.40903463028482356, 48.52187500034140299, 47.42413220539093999 ) ) ;
#7960 = CARTESIAN_POINT ( 'NONE',  ( -7.500000000000000000, 25.00000000000000355, -39.29058411375427795 ) ) ;
#7961 = ORIENTED_EDGE ( 'NONE', *, *, #12301, .F. ) ;
#7962 = CARTESIAN_POINT ( 'NONE',  ( 15.40903463028482356, 46.52187500034139589, 47.42413220539093999 ) ) ;
#7963 = EDGE_LOOP ( 'NONE', ( #15541, #12355, #11633, #10508 ) ) ;
#7964 = CARTESIAN_POINT ( 'NONE',  ( 17.28626291527370284, 40.00000000000000711, -18.64048258526062085 ) ) ;
#7965 = EDGE_LOOP ( 'NONE', ( #9323, #2918, #4481, #7718, #2110 ) ) ;
#7966 = ORIENTED_EDGE ( 'NONE', *, *, #6754, .F. ) ;
#7967 =( BOUNDED_CURVE ( )  B_SPLINE_CURVE ( 3, ( #13739, #14724, #9927, #16237 ),
 .UNSPECIFIED., .F., .F. ) 
 B_SPLINE_CURVE_WITH_KNOTS ( ( 4, 4 ),
 ( 5.700094519411438299, 6.866276094947727948 ),
 .UNSPECIFIED. ) 
 CURVE ( )  GEOMETRIC_REPRESENTATION_ITEM ( )  RATIONAL_B_SPLINE_CURVE ( ( 1.000000000000000000, 0.8898432210558864242, 0.8898432210558864242, 1.000000000000000000 ) ) 
 REPRESENTATION_ITEM ( '' )  );
#7968 = ADVANCED_FACE ( 'NONE', ( #14325 ), #5299, .T. ) ;
#7969 = DIRECTION ( 'NONE',  ( -0.000000000000000000, -1.000000000000000000, -0.000000000000000000 ) ) ;
#7970 = CARTESIAN_POINT ( 'NONE',  ( 4.898587196589413026E-15, 25.00000000000000355, 40.00000000000000000 ) ) ;
#7971 = LINE ( 'NONE', #13043, #15657 ) ;
#7972 = CARTESIAN_POINT ( 'NONE',  ( 49.99999999999999289, 25.10000000000000142, -16.24598481164532160 ) ) ;
#7973 = CARTESIAN_POINT ( 'NONE',  ( -40.34137639590981905, 41.65937500034139873, -29.30972558990011478 ) ) ;
#7974 = CARTESIAN_POINT ( 'NONE',  ( 30.90169943749475223, 48.48125000068279888, 42.53254041760199300 ) ) ;
#7975 = DIRECTION ( 'NONE',  ( -6.938893903907231459E-18, 1.000000000000000000, 5.551115123125782702E-17 ) ) ;
#7976 = CARTESIAN_POINT ( 'NONE',  ( -3.111920190527341144E-15, 45.50000000000000000, -50.00000000000000000 ) ) ;
#7977 = DIRECTION ( 'NONE',  ( 0.000000000000000000, 1.000000000000000000, 0.000000000000000000 ) ) ;
#7978 = CARTESIAN_POINT ( 'NONE',  ( -40.45084971874737789, 43.58125000068280031, -29.38926261462365730 ) ) ;
#7979 = CARTESIAN_POINT ( 'NONE',  ( -16.15689471564406432, 27.22396221095493729, 101.6666710451724214 ) ) ;
#7980 = CARTESIAN_POINT ( 'NONE',  ( 30.90169943749475223, 46.48125000068280599, 42.53254041760199300 ) ) ;
#7981 = LINE ( 'NONE', #5269, #4327 ) ;
#7982 = ORIENTED_EDGE ( 'NONE', *, *, #496, .F. ) ;
#7983 = CARTESIAN_POINT ( 'NONE',  ( 30.81806926056962936, 35.15937500034139873, -42.41743335407647209 ) ) ;
#7984 = ORIENTED_EDGE ( 'NONE', *, *, #11252, .T. ) ;
#7985 = EDGE_LOOP ( 'NONE', ( #12469, #11146, #12626, #15934 ) ) ;
#7986 = CARTESIAN_POINT ( 'NONE',  ( 15.45084971874736723, 43.39999999999999858, -47.55282581475768211 ) ) ;
#7987 = LINE ( 'NONE', #13224, #4719 ) ;
#7988 = CARTESIAN_POINT ( 'NONE',  ( -30.81806926056962226, 22.15937500034139873, 42.41743335407647919 ) ) ;
#7989 = VERTEX_POINT ( 'NONE', #6620 ) ;
#7990 = PRODUCT_DEFINITION_SHAPE ( 'NONE', 'NONE',  #9149 ) ;
#7991 = DIRECTION ( 'NONE',  ( -0.000000000000000000, -0.000000000000000000, -1.000000000000000000 ) ) ;
#7992 = LINE ( 'NONE', #11899, #4688 ) ;
#7993 = CARTESIAN_POINT ( 'NONE',  ( 0.000000000000000000, 20.00000000000000355, 0.000000000000000000 ) ) ;
#7994 = CARTESIAN_POINT ( 'NONE',  ( 15.40903463028482356, 26.52187500034139589, 47.42413220539093999 ) ) ;
#7995 = CARTESIAN_POINT ( 'NONE',  ( 0.000000000000000000, 102.0000000000000142, 5.000000000000000000 ) ) ;
#7996 = DIRECTION ( 'NONE',  ( 0.000000000000000000, 0.000000000000000000, -1.000000000000000000 ) ) ;
#7997 = CARTESIAN_POINT ( 'NONE',  ( -46.31917516190693362, 20.00000000000000355, 18.46674513801226425 ) ) ;
#7998 = CARTESIAN_POINT ( 'NONE',  ( -49.86468353125000164, 27.92187500034139447, 0.000000000000000000 ) ) ;
#7999 = LINE ( 'NONE', #13073, #12387 ) ;
#8000 = CARTESIAN_POINT ( 'NONE',  ( 30.90169943749475578, 32.70000000000000284, 42.53254041760200010 ) ) ;
#8001 = CARTESIAN_POINT ( 'NONE',  ( -3.210462471511496205E-15, 31.35937500034139092, -52.43083105670540789 ) ) ;
#8002 = CARTESIAN_POINT ( 'NONE',  ( -0.5000000000000000000, 242.0000000000000284, -47.99999999999999289 ) ) ;
#8003 = VERTEX_POINT ( 'NONE', #7080 ) ;
#8004 = CARTESIAN_POINT ( 'NONE',  ( 49.86468353125001585, 28.75937500034139305, 16.20201782572375038 ) ) ;
#8005 = ORIENTED_EDGE ( 'NONE', *, *, #11699, .T. ) ;
#8006 = DIRECTION ( 'NONE',  ( -0.000000000000000000, -1.000000000000000000, -0.000000000000000000 ) ) ;
#8007 = ADVANCED_BREP_SHAPE_REPRESENTATION ( '', ( #8709, #15812 ), #3617 ) ;
#8008 = CARTESIAN_POINT ( 'NONE',  ( 9.631387414534489405E-15, 42.35937500034140157, 52.43083105670540789 ) ) ;
#8009 = DIRECTION ( 'NONE',  ( 0.000000000000000000, 1.000000000000000000, 0.000000000000000000 ) ) ;
#8010 = CARTESIAN_POINT ( 'NONE',  ( 20.31983351293711237, 285.7035871579557238, 7.659916756470837917 ) ) ;
#8011 = CARTESIAN_POINT ( 'NONE',  ( -20.51073895446497986, 285.3889217077648368, 7.755369477226736308 ) ) ;
#8012 = CARTESIAN_POINT ( 'NONE',  ( -49.86468353124999453, 36.02187500034139589, 16.20201782572377525 ) ) ;
#8013 = CARTESIAN_POINT ( 'NONE',  ( 49.86468353125000164, 34.85937500034140157, -6.106662507704105588E-15 ) ) ;
#8014 = CARTESIAN_POINT ( 'NONE',  ( -4.336808689942015887E-17, 307.0000000000000568, -2.499999999999999112 ) ) ;
#8015 = CARTESIAN_POINT ( 'NONE',  ( 50.00000000000000711, 42.89999999999999858, 16.24598481164530739 ) ) ;
#8016 = CARTESIAN_POINT ( 'NONE',  ( -40.45084971874737789, 23.58125000068280031, -29.38926261462365730 ) ) ;
#8017 = CARTESIAN_POINT ( 'NONE',  ( 40.34137639590981195, 43.12187500034139731, -29.30972558990011834 ) ) ;
#8018 = CARTESIAN_POINT ( 'NONE',  ( 49.86468353124999453, 25.02187500034139589, -16.20201782572376459 ) ) ;
#8019 = B_SPLINE_CURVE_WITH_KNOTS ( 'NONE', 3,
 ( #10462, #9221, #6572, #14189 ),
 .UNSPECIFIED., .F., .F.,
 ( 4, 4 ),
 ( 0.009967034006374431848, 0.01711986125270675840 ),
 .UNSPECIFIED. ) ;
#8020 = CARTESIAN_POINT ( 'NONE',  ( 15.40903463028482356, 46.45937500034139589, 47.42413220539093999 ) ) ;
#8021 = ORIENTED_EDGE ( 'NONE', *, *, #5809, .F. ) ;
#8022 = CARTESIAN_POINT ( 'NONE',  ( 49.99999999999999289, 30.88125000068279391, -16.24598481164532160 ) ) ;
#8023 = ORIENTED_EDGE ( 'NONE', *, *, #3983, .T. ) ;
#8024 = LINE ( 'NONE', #6801, #7862 ) ;
#8025 = CARTESIAN_POINT ( 'NONE',  ( -2.547328955960238000E-13, 30.28125000068279604, 49.99999999999999289 ) ) ;
#8026 = EDGE_CURVE ( 'NONE', #4340, #11702, #9346, .T. ) ;
#8027 = CIRCLE ( 'NONE', #856, 40.00000000000000000 ) ;
#8028 = CARTESIAN_POINT ( 'NONE',  ( -49.93234176562499727, 49.82031250051209526, 0.000000000000000000 ) ) ;
#8029 = CARTESIAN_POINT ( 'NONE',  ( -40.34137639590981195, 48.12187500034139731, 29.30972558990012189 ) ) ;
#8030 = CARTESIAN_POINT ( 'NONE',  ( -49.86468353125000164, 27.85937500034139447, 0.000000000000000000 ) ) ;
#8031 = DIRECTION ( 'NONE',  ( 0.000000000000000000, 1.000000000000000000, 0.000000000000000000 ) ) ;
#8032 = CARTESIAN_POINT ( 'NONE',  ( 30.81806926056964002, 40.62187500034139731, 42.41743335407646498 ) ) ;
#8033 = DIRECTION ( 'NONE',  ( 1.000000000000000000, 0.000000000000000000, 0.000000000000000000 ) ) ;
#8034 = EDGE_CURVE ( 'NONE', #1788, #4999, #2772, .T. ) ;
#8035 = EDGE_CURVE ( 'NONE', #6499, #16264, #6913, .T. ) ;
#8036 = CARTESIAN_POINT ( 'NONE',  ( -30.81806926056963292, 45.62187500034139020, -42.41743335407647209 ) ) ;
#8037 = CARTESIAN_POINT ( 'NONE',  ( -3.111920190527341144E-15, 45.28125000068279604, -50.00000000000000000 ) ) ;
#8038 = ORIENTED_EDGE ( 'NONE', *, *, #9262, .T. ) ;
#8039 = CONICAL_SURFACE ( 'NONE', #12565, 16.50000000000000711, 0.7853981633974447263 ) ;
#8040 = EDGE_CURVE ( 'NONE', #11148, #8474, #15577, .T. ) ;
#8041 = CARTESIAN_POINT ( 'NONE',  ( 15.40903463028481113, 49.32187500034139305, -47.42413220539094709 ) ) ;
#8042 = EDGE_LOOP ( 'NONE', ( #11410, #15131, #6990 ) ) ;
#8043 = CARTESIAN_POINT ( 'NONE',  ( 0.000000000000000000, 55.00000000000000711, 0.000000000000000000 ) ) ;
#8044 = ORIENTED_EDGE ( 'NONE', *, *, #12039, .F. ) ;
#8045 = CARTESIAN_POINT ( 'NONE',  ( -5.000000000000000000, 92.00000000000001421, 0.000000000000000000 ) ) ;
#8046 = DIRECTION ( 'NONE',  ( 0.7431448254773955764, -0.6691306063588567943, 0.000000000000000000 ) ) ;
#8047 = FACE_OUTER_BOUND ( 'NONE', #13198, .T. ) ;
#8048 = CARTESIAN_POINT ( 'NONE',  ( 50.00000000000000000, 25.00000000000000000, -6.123233995736766085E-15 ) ) ;
#8049 = CARTESIAN_POINT ( 'NONE',  ( -49.86468353124999453, 45.95937500034138878, 16.20201782572377525 ) ) ;
#8050 = CARTESIAN_POINT ( 'NONE',  ( -40.45084971874737789, 25.58125000068279675, -29.38926261462365730 ) ) ;
#8051 = CARTESIAN_POINT ( 'NONE',  ( 0.000000000000000000, 22.50000000000000000, 102.0000000000000142 ) ) ;
#8052 = VECTOR ( 'NONE', #15774, 1000.000000000000000 ) ;
#8053 = CARTESIAN_POINT ( 'NONE',  ( 0.000000000000000000, 55.00000000000000711, 0.000000000000000000 ) ) ;
#8054 = CARTESIAN_POINT ( 'NONE',  ( 9.574901606694759531E-15, 52.00000000000001421, 34.99999999999999289 ) ) ;
#8055 = CARTESIAN_POINT ( 'NONE',  ( 15.45084971874736723, 33.18125000068279462, -47.55282581475768211 ) ) ;
#8056 = CARTESIAN_POINT ( 'NONE',  ( 16.47405064338586200, 27.32701241865550656, 101.3333374614808662 ) ) ;
#8057 = CARTESIAN_POINT ( 'NONE',  ( 0.000000000000000000, 193.4213562373095385, -50.00000000000000000 ) ) ;
#8058 = FACE_OUTER_BOUND ( 'NONE', #4779, .T. ) ;
#8059 = VERTEX_POINT ( 'NONE', #11674 ) ;
#8060 =( BOUNDED_CURVE ( )  B_SPLINE_CURVE ( 2, ( #8279, #14419, #8112, #11859, #7955, #9449, #11939, #10860, #5475, #1629, #4224, #5634, #12099 ),
 .UNSPECIFIED., .F., .T. ) 
 B_SPLINE_CURVE_WITH_KNOTS ( ( 3, 2, 2, 2, 2, 2, 3 ),
 ( 0.3166666666666667074, 0.3200000000000000067, 0.3266666666666666607, 0.3333333333333333148, 0.3400000000000000244, 0.3466666666666666785, 0.3500000000000000333 ),
 .UNSPECIFIED. ) 
 CURVE ( )  GEOMETRIC_REPRESENTATION_ITEM ( )  RATIONAL_B_SPLINE_CURVE ( ( 0.9755282581475768211, 0.9755282581475770431, 1.000000000000000000, 0.9510565162951535312, 1.000000000000000000, 0.9510565162951535312, 1.000000000000000000, 0.9510565162951535312, 1.000000000000000000, 0.9510565162951535312, 1.000000000000000000, 0.9755282581475765991, 0.9755282581475768211 ) ) 
 REPRESENTATION_ITEM ( '' )  );
#8061 = CARTESIAN_POINT ( 'NONE',  ( -40.34137639590981905, 39.65937500034139873, -29.30972558990011478 ) ) ;
#8062 = VERTEX_POINT ( 'NONE', #13083 ) ;
#8063 = ORIENTED_EDGE ( 'NONE', *, *, #10590, .F. ) ;
#8064 = AXIS2_PLACEMENT_3D ( 'NONE', #1576, #7977, #13051 ) ;
#8065 = CARTESIAN_POINT ( 'NONE',  ( -49.99999999999999289, 49.68125000068279462, -16.24598481164531449 ) ) ;
#8066 = DIRECTION ( 'NONE',  ( -0.000000000000000000, -0.000000000000000000, 1.000000000000000000 ) ) ;
#8067 = CARTESIAN_POINT ( 'NONE',  ( -15.40903463028481646, 21.45937500034139589, -47.42413220539093999 ) ) ;
#8068 = ORIENTED_EDGE ( 'NONE', *, *, #11483, .T. ) ;
#8069 = DIRECTION ( 'NONE',  ( 0.1045284632676570929, -0.9945218953682730678, 0.000000000000000000 ) ) ;
#8070 = CARTESIAN_POINT ( 'NONE',  ( 50.00000000000000000, 23.00000000000000355, -6.123233995736766085E-15 ) ) ;
#8071 = CARTESIAN_POINT ( 'NONE',  ( 30.00000000000000000, 282.0000000000000000, 12.50000000000000178 ) ) ;
#8072 = CARTESIAN_POINT ( 'NONE',  ( 49.86468353125000164, 30.92187500034139802, -6.106662507704105588E-15 ) ) ;
#8073 = DIRECTION ( 'NONE',  ( 0.08715574274765797158, 0.9961946980917455452, -0.000000000000000000 ) ) ;
#8074 = CARTESIAN_POINT ( 'NONE',  ( 17.50000000000000000, 22.50000000000000355, 94.42467108177066848 ) ) ;
#8075 = CARTESIAN_POINT ( 'NONE',  ( -47.55097084096128413, 20.00000000000001066, 15.01398062573002612 ) ) ;
#8076 = CIRCLE ( 'NONE', #8871, 2.000000000000000000 ) ;
#8077 = CARTESIAN_POINT ( 'NONE',  ( 9.631387414534489405E-15, 26.42187500034139447, 52.43083105670540789 ) ) ;
#8078 = CARTESIAN_POINT ( 'NONE',  ( -50.00000000000000000, 22.00000000000000355, 0.000000000000000000 ) ) ;
#8079 = VECTOR ( 'NONE', #7701, 1000.000000000000000 ) ;
#8080 = CARTESIAN_POINT ( 'NONE',  ( -40.45084971874737789, 35.79999999999999716, -29.38926261462365730 ) ) ;
#8081 = CARTESIAN_POINT ( 'NONE',  ( -30.81806926056962226, 32.15937500034139873, 42.41743335407647919 ) ) ;
#8082 = DIRECTION ( 'NONE',  ( -1.000000000000000000, 0.000000000000000000, 0.000000000000000000 ) ) ;
#8083 = ORIENTED_EDGE ( 'NONE', *, *, #1120, .T. ) ;
#8084 = CARTESIAN_POINT ( 'NONE',  ( -49.86468353124999453, 27.95937500034139944, 16.20201782572377169 ) ) ;
#8085 = EDGE_CURVE ( 'NONE', #15764, #12729, #8090, .T. ) ;
#8086 = VERTEX_POINT ( 'NONE', #11830 ) ;
#8087 = DIRECTION ( 'NONE',  ( 0.000000000000000000, 1.000000000000000000, 0.000000000000000000 ) ) ;
#8088 = CARTESIAN_POINT ( 'NONE',  ( -30.81806926056962226, 42.15937500034139163, 42.41743335407647919 ) ) ;
#8089 = AXIS2_PLACEMENT_3D ( 'NONE', #1251, #6343, #11409 ) ;
#8090 = LINE ( 'NONE', #1688, #14180 ) ;
#8091 = CARTESIAN_POINT ( 'NONE',  ( -30.81806926056962226, 20.22187500034139163, 42.41743335407647919 ) ) ;
#8092 = CARTESIAN_POINT ( 'NONE',  ( -26.40559293885987913, 283.2826504366940981, 8.905592938858424290 ) ) ;
#8093 = CARTESIAN_POINT ( 'NONE',  ( 49.86468353125000164, 36.92187500034140157, -6.106662507704105588E-15 ) ) ;
#8094 = CARTESIAN_POINT ( 'NONE',  ( 15.40903463028482356, 38.45937500034139589, 47.42413220539093999 ) ) ;
#8095 = DIRECTION ( 'NONE',  ( 1.000000000000000000, 0.000000000000000000, 0.000000000000000000 ) ) ;
#8096 = CARTESIAN_POINT ( 'NONE',  ( -40.45084971874737789, 43.80000000000000426, -29.38926261462365730 ) ) ;
#8097 = CARTESIAN_POINT ( 'NONE',  ( 40.45084971874737789, 22.58125000068279675, 29.38926261462365375 ) ) ;
#8098 = CARTESIAN_POINT ( 'NONE',  ( -49.86468353125000164, 45.92187500034139447, 0.000000000000000000 ) ) ;
#8099 = AXIS2_PLACEMENT_3D ( 'NONE', #11523, #6217, #7625 ) ;
#8100 = CARTESIAN_POINT ( 'NONE',  ( 15.40903463028481113, 25.32187500034139660, -47.42413220539094709 ) ) ;
#8101 = CARTESIAN_POINT ( 'NONE',  ( -49.86468353124999453, 47.75937500034139305, -16.20201782572375393 ) ) ;
#8102 = ORIENTED_EDGE ( 'NONE', *, *, #13920, .T. ) ;
#8103 = CARTESIAN_POINT ( 'NONE',  ( -3.219174618344376363E-15, 29.28125000068279604, -52.57311121191334990 ) ) ;
#8104 = ORIENTED_EDGE ( 'NONE', *, *, #12874, .F. ) ;
#8105 = VECTOR ( 'NONE', #9692, 1000.000000000000000 ) ;
#8106 = DIRECTION ( 'NONE',  ( -1.000000000000000000, 0.000000000000000000, -0.000000000000000000 ) ) ;
#8107 = AXIS2_PLACEMENT_3D ( 'NONE', #13359, #8784, #7705 ) ;
#8108 = CARTESIAN_POINT ( 'NONE',  ( 40.45084971874737789, 30.58125000068279675, 29.38926261462365375 ) ) ;
#8109 = CARTESIAN_POINT ( 'NONE',  ( 15.40903463028481113, 45.32187500034140015, -47.42413220539094709 ) ) ;
#8110 = CARTESIAN_POINT ( 'NONE',  ( 30.81806926056962936, 27.15937500034139163, -42.41743335407647209 ) ) ;
#8111 = MECHANICAL_DESIGN_GEOMETRIC_PRESENTATION_REPRESENTATION (  '', ( #12359 ), #8644 ) ;
#8112 = CARTESIAN_POINT ( 'NONE',  ( -15.45084971874736368, 40.18125000068280173, 47.55282581475768211 ) ) ;
#8113 = CARTESIAN_POINT ( 'NONE',  ( 40.34137639590981905, 40.72187500034139873, 29.30972558990010768 ) ) ;
#8114 = AXIS2_PLACEMENT_3D ( 'NONE', #1613, #11756, #11836 ) ;
#8115 = DIRECTION ( 'NONE',  ( 1.000000000000000000, 0.000000000000000000, 0.000000000000000000 ) ) ;
#8116 = CARTESIAN_POINT ( 'NONE',  ( -49.86468353124999453, 46.02187500034140299, 16.20201782572377525 ) ) ;
#8117 = VECTOR ( 'NONE', #137, 999.9999999999998863 ) ;
#8118 = CARTESIAN_POINT ( 'NONE',  ( 50.00000000000000000, 31.00000000000000355, -6.123233995736766085E-15 ) ) ;
#8119 = VECTOR ( 'NONE', #3540, 1000.000000000000000 ) ;
#8120 = AXIS2_PLACEMENT_3D ( 'NONE', #1668, #10493, #10823 ) ;
#8121 = VERTEX_POINT ( 'NONE', #439 ) ;
#8122 = AXIS2_PLACEMENT_3D ( 'NONE', #6348, #11415, #2673 ) ;
#8123 = EDGE_CURVE ( 'NONE', #172, #5355, #5964, .T. ) ;
#8124 = CARTESIAN_POINT ( 'NONE',  ( 9.631387414534489405E-15, 40.42187500034138736, 52.43083105670540789 ) ) ;
#8125 = PRODUCT ( 'Lid Filler Cap _ Measuring Cup', 'Lid Filler Cap _ Measuring Cup', '', ( #6727 ) ) ;
#8126 = EDGE_LOOP ( 'NONE', ( #918, #6760, #16123, #15706 ) ) ;
#8127 = ORIENTED_EDGE ( 'NONE', *, *, #9559, .T. ) ;
#8128 = CARTESIAN_POINT ( 'NONE',  ( 50.00000000000000000, 21.00000000000000000, -6.123233995736766085E-15 ) ) ;
#8129 = EDGE_CURVE ( 'NONE', #2703, #14669, #11065, .T. ) ;
#8130 = LINE ( 'NONE', #8045, #1786 ) ;
#8131 = CARTESIAN_POINT ( 'NONE',  ( 0.000000000000000000, 22.50000000000000000, 102.0000000000000142 ) ) ;
#8132 = EDGE_CURVE ( 'NONE', #11630, #8883, #1698, .T. ) ;
#8133 = LINE ( 'NONE', #3056, #8490 ) ;
#8134 = CARTESIAN_POINT ( 'NONE',  ( 40.45084971874737079, 27.20000000000000284, -29.38926261462366440 ) ) ;
#8135 = CIRCLE ( 'NONE', #15278, 63.16733765196516970 ) ;
#8136 = CARTESIAN_POINT ( 'NONE',  ( 49.86468353125000164, 44.85937500034140157, -6.106662507704105588E-15 ) ) ;
#8137 = AXIS2_PLACEMENT_3D ( 'NONE', #8748, #10008, #15065 ) ;
#8138 = COLOUR_RGB ( '', 0.09019608, 0.27058824, 0.51372549) ;
#8139 = CARTESIAN_POINT ( 'NONE',  ( 8.446640517145639571E-15, 48.28125000068279604, 50.00000000000000000 ) ) ;
#8140 = CARTESIAN_POINT ( 'NONE',  ( 3.407225380398686276, 31.38205016914263723, 101.0000000000000000 ) ) ;
#8141 = AXIS2_PLACEMENT_3D ( 'NONE', #591, #3262, #11749 ) ;
#8142 = DIRECTION ( 'NONE',  ( -0.000000000000000000, -1.000000000000000000, -0.000000000000000000 ) ) ;
#8143 = ADVANCED_FACE ( 'NONE', ( #4762 ), #2402, .F. ) ;
#8144 = CARTESIAN_POINT ( 'NONE',  ( 0.000000000000000000, 20.00000000000000355, 50.00000000000000000 ) ) ;
#8145 = CARTESIAN_POINT ( 'NONE',  ( -50.00000000000000000, 33.78125000068280315, 0.000000000000000000 ) ) ;
#8146 = CARTESIAN_POINT ( 'NONE',  ( -15.83973438765502451, 27.12091057352761325, 102.0000000000000142 ) ) ;
#8147 = CARTESIAN_POINT ( 'NONE',  ( 40.45084971874737789, 20.58125000068280031, 29.38926261462365375 ) ) ;
#8148 = CARTESIAN_POINT ( 'NONE',  ( -11.92169313911859341, 33.90715708214334256, 102.0000000000000142 ) ) ;
#8149 = ORIENTED_EDGE ( 'NONE', *, *, #16173, .T. ) ;
#8150 = EDGE_CURVE ( 'NONE', #871, #9545, #8480, .T. ) ;
#8151 = CARTESIAN_POINT ( 'NONE',  ( -15.40903463028480580, 30.25937500034140015, 47.42413220539094709 ) ) ;
#8152 = VECTOR ( 'NONE', #13741, 1000.000000000000000 ) ;
#8153 = VERTEX_POINT ( 'NONE', #11231 ) ;
#8154 = VERTEX_POINT ( 'NONE', #9898 ) ;
#8155 = VECTOR ( 'NONE', #10819, 1000.000000000000000 ) ;
#8156 = CARTESIAN_POINT ( 'NONE',  ( 50.00000000000000000, 43.00000000000000000, -6.123233995736766085E-15 ) ) ;
#8157 = DIRECTION ( 'NONE',  ( 0.000000000000000000, 0.000000000000000000, 1.000000000000000000 ) ) ;
#8158 = CARTESIAN_POINT ( 'NONE',  ( 15.40903463028482356, 24.45937500034139589, 47.42413220539093999 ) ) ;
#8159 = EDGE_LOOP ( 'NONE', ( #7133, #11353, #12961, #15155, #16307, #12539, #13379, #16396, #11129, #15997, #10120, #13435, #6076, #6738, #3493, #4313, #9887, #1822 ) ) ;
#8160 = DIRECTION ( 'NONE',  ( 0.4067366430758010964, -0.9135454576426004225, 0.000000000000000000 ) ) ;
#8161 = CARTESIAN_POINT ( 'NONE',  ( 40.45084971874737789, 22.80000000000000071, 29.38926261462365375 ) ) ;
#8162 = CARTESIAN_POINT ( 'NONE',  ( 19.99999999999999289, 287.0000000000000568, 7.500000000000002665 ) ) ;
#8163 = CARTESIAN_POINT ( 'NONE',  ( -3.210462471511496205E-15, 29.42187500034139447, -52.43083105670540789 ) ) ;
#8164 = FACE_OUTER_BOUND ( 'NONE', #8903, .T. ) ;
#8165 = EDGE_CURVE ( 'NONE', #11431, #2476, #13708, .T. ) ;
#8166 = CARTESIAN_POINT ( 'NONE',  ( 40.45084971874737079, 47.20000000000000284, -29.38926261462366440 ) ) ;
#8167 = CARTESIAN_POINT ( 'NONE',  ( -47.88920767661647204, 19.99999999999999645, 13.89741811465869503 ) ) ;
#8168 = CARTESIAN_POINT ( 'NONE',  ( -3.210462471511496205E-15, 23.42187500034139447, -52.43083105670540789 ) ) ;
#8169 =( BOUNDED_CURVE ( )  B_SPLINE_CURVE ( 2, ( #651, #3241, #8314, #746, #1068, #7562, #1315, #13867, #15118, #12633, #8723, #14036, #1235 ),
 .UNSPECIFIED., .F., .T. ) 
 B_SPLINE_CURVE_WITH_KNOTS ( ( 3, 2, 2, 2, 2, 2, 3 ),
 ( 0.3833333333333333592, 0.3866666666666666585, 0.3933333333333333126, 0.4000000000000000222, 0.4066666666666666763, 0.4133333333333333304, 0.4166666666666666852 ),
 .UNSPECIFIED. ) 
 CURVE ( )  GEOMETRIC_REPRESENTATION_ITEM ( )  RATIONAL_B_SPLINE_CURVE ( ( 0.9755282581475768211, 0.9755282581475770431, 1.000000000000000000, 0.9510565162951535312, 1.000000000000000000, 0.9510565162951535312, 1.000000000000000000, 0.9510565162951535312, 1.000000000000000000, 0.9510565162951535312, 1.000000000000000000, 0.9755282581475765991, 0.9755282581475768211 ) ) 
 REPRESENTATION_ITEM ( '' )  );
#8170 = CARTESIAN_POINT ( 'NONE',  ( -30.90169943749473447, 22.29999999999999716, 42.53254041760200721 ) ) ;
#8171 = CARTESIAN_POINT ( 'NONE',  ( -15.45084971874736368, 32.39999999999999858, 47.55282581475768211 ) ) ;
#8172 = CARTESIAN_POINT ( 'NONE',  ( -40.34137639590981905, 25.65937500034139518, -29.30972558990011478 ) ) ;
#8173 = EDGE_CURVE ( 'NONE', #4002, #9078, #825, .T. ) ;
#8174 = LINE ( 'NONE', #3797, #4883 ) ;
#8175 = ORIENTED_EDGE ( 'NONE', *, *, #9362, .T. ) ;
#8176 = CARTESIAN_POINT ( 'NONE',  ( -49.86468353124999453, 31.75937500034140015, -16.20201782572375393 ) ) ;
#8177 = ORIENTED_EDGE ( 'NONE', *, *, #10399, .T. ) ;
#8178 = LINE ( 'NONE', #10600, #15299 ) ;
#8179 = CARTESIAN_POINT ( 'NONE',  ( -30.81806926056963292, 41.55937500034139731, -42.41743335407647209 ) ) ;
#8180 = EDGE_CURVE ( 'NONE', #5251, #326, #4110, .T. ) ;
#8181 = CARTESIAN_POINT ( 'NONE',  ( 21.01167039530811209, 284.7842439685853719, 8.005835197659997959 ) ) ;
#8182 = CARTESIAN_POINT ( 'NONE',  ( 0.000000000000000000, 32.49999999999998579, -40.00000000000000000 ) ) ;
#8183 = CARTESIAN_POINT ( 'NONE',  ( 9.631387414534489405E-15, 32.42187500034139447, 52.43083105670540789 ) ) ;
#8184 = CARTESIAN_POINT ( 'NONE',  ( -30.81806926056963292, 35.55937500034139020, -42.41743335407646498 ) ) ;
#8185 = LINE ( 'NONE', #15492, #12101 ) ;
#8186 = CARTESIAN_POINT ( 'NONE',  ( -3.210462471511496205E-15, 31.42187500034139447, -52.43083105670540789 ) ) ;
#8187 = CARTESIAN_POINT ( 'NONE',  ( 50.00000000000000000, 43.00000000000000000, -6.123233995736766085E-15 ) ) ;
#8188 = AXIS2_PLACEMENT_3D ( 'NONE', #3974, #14101, #11296 ) ;
#8189 = CARTESIAN_POINT ( 'NONE',  ( 40.45084971874737079, 20.98125000068279888, -29.38926261462366440 ) ) ;
#8190 = CARTESIAN_POINT ( 'NONE',  ( 9.631387414534489405E-15, 46.42187500034139447, 52.43083105670540789 ) ) ;
#8191 = CARTESIAN_POINT ( 'NONE',  ( 49.86468353125001585, 20.82187500034140015, 16.20201782572375038 ) ) ;
#8192 = VERTEX_POINT ( 'NONE', #6238 ) ;
#8193 = CARTESIAN_POINT ( 'NONE',  ( -15.40903463028480580, 46.25937500034140015, 47.42413220539094709 ) ) ;
#8194 = ORIENTED_EDGE ( 'NONE', *, *, #8034, .F. ) ;
#8195 = B_SPLINE_CURVE_WITH_KNOTS ( 'NONE', 3,
 ( #2793, #12946, #1550, #6643 ),
 .UNSPECIFIED., .F., .F.,
 ( 4, 4 ),
 ( 2.829004760673920638E-07, 0.001414802801989366136 ),
 .UNSPECIFIED. ) ;
#8196 = CARTESIAN_POINT ( 'NONE',  ( -15.45084971874737256, 31.38125000068280102, -47.55282581475767500 ) ) ;
#8197 = ORIENTED_EDGE ( 'NONE', *, *, #5536, .F. ) ;
#8198 = CYLINDRICAL_SURFACE ( 'NONE', #7596, 50.00000000000000000 ) ;
#8199 = CARTESIAN_POINT ( 'NONE',  ( 7.919222016226940219, 33.22999571913595673, -49.99999999999996447 ) ) ;
#8200 = CARTESIAN_POINT ( 'NONE',  ( -30.81806926056962226, 38.22187500034139873, 42.41743335407647209 ) ) ;
#8201 = CARTESIAN_POINT ( 'NONE',  ( 49.86468353124999453, 22.95937500034139589, -16.20201782572376459 ) ) ;
#8202 = DIRECTION ( 'NONE',  ( -0.8660254037844433705, 0.4999999999999918399, 0.000000000000000000 ) ) ;
#8203 = EDGE_CURVE ( 'NONE', #7781, #6366, #9740, .T. ) ;
#8204 = CARTESIAN_POINT ( 'NONE',  ( 40.45084971874737079, 35.20000000000000284, -29.38926261462366440 ) ) ;
#8205 = CARTESIAN_POINT ( 'NONE',  ( -49.86468353125000164, 49.92187500034140157, 0.000000000000000000 ) ) ;
#8206 = FACE_OUTER_BOUND ( 'NONE', #7342, .T. ) ;
#8207 = ORIENTED_EDGE ( 'NONE', *, *, #4087, .T. ) ;
#8208 = CARTESIAN_POINT ( 'NONE',  ( 40.34137639590981905, 44.72187500034139163, 29.30972558990010768 ) ) ;
#8209 = VERTEX_POINT ( 'NONE', #2232 ) ;
#8210 = EDGE_LOOP ( 'NONE', ( #14655, #7860, #9872, #9546 ) ) ;
#8211 = ADVANCED_FACE ( 'NONE', ( #12475 ), #15038, .T. ) ;
#8212 = CARTESIAN_POINT ( 'NONE',  ( 0.5000000000000009992, 31.99999999999998579, 102.0000000000000142 ) ) ;
#8213 = CARTESIAN_POINT ( 'NONE',  ( -12.67046914267499069, 34.58135802401869086, 101.0000000000000000 ) ) ;
#8214 = CARTESIAN_POINT ( 'NONE',  ( 0.000000000000000000, 193.4213562373095385, 0.000000000000000000 ) ) ;
#8215 = CARTESIAN_POINT ( 'NONE',  ( 49.99999999999999289, 21.09999999999999787, -16.24598481164532160 ) ) ;
#8216 = VECTOR ( 'NONE', #1985, 1000.000000000000000 ) ;
#8217 = CARTESIAN_POINT ( 'NONE',  ( -40.34137639590981195, 44.05937500034139731, 29.30972558990012189 ) ) ;
#8218 = CARTESIAN_POINT ( 'NONE',  ( -49.86468353125000164, 49.85937500034139447, 0.000000000000000000 ) ) ;
#8219 = CARTESIAN_POINT ( 'NONE',  ( 0.000000000000000000, 193.4213562373095385, -50.00000000000000000 ) ) ;
#8220 = CARTESIAN_POINT ( 'NONE',  ( -15.45084971874736368, 34.18125000068279462, 47.55282581475768211 ) ) ;
#8221 = SURFACE_STYLE_USAGE ( .BOTH. , #6071 ) ;
#8222 = LINE ( 'NONE', #13288, #14422 ) ;
#8223 = CARTESIAN_POINT ( 'NONE',  ( 0.000000000000000000, 52.00000000000000711, 0.000000000000000000 ) ) ;
#8224 = CARTESIAN_POINT ( 'NONE',  ( -20.00000000000000355, 287.0000000000000568, 2.500000000000000444 ) ) ;
#8225 = FACE_OUTER_BOUND ( 'NONE', #13155, .T. ) ;
#8226 = EDGE_CURVE ( 'NONE', #7784, #4024, #1261, .T. ) ;
#8227 = VERTEX_POINT ( 'NONE', #12223 ) ;
#8228 = CARTESIAN_POINT ( 'NONE',  ( 49.86468353125000164, 28.85937500034139802, -6.106662507704105588E-15 ) ) ;
#8229 = VECTOR ( 'NONE', #6239, 1000.000000000000000 ) ;
#8230 = EDGE_LOOP ( 'NONE', ( #8251, #15609, #5953, #3538 ) ) ;
#8231 = EDGE_LOOP ( 'NONE', ( #6039, #15343 ) ) ;
#8232 = ORIENTED_EDGE ( 'NONE', *, *, #1475, .T. ) ;
#8233 = CARTESIAN_POINT ( 'NONE',  ( 9.657523855033129090E-15, 46.28125000068279604, 52.57311121191334990 ) ) ;
#8234 = DIRECTION ( 'NONE',  ( 0.000000000000000000, 0.000000000000000000, 1.000000000000000000 ) ) ;
#8235 = CARTESIAN_POINT ( 'NONE',  ( 40.34137639590981905, 24.65937500034139873, 29.30972558990010768 ) ) ;
#8236 = EDGE_LOOP ( 'NONE', ( #14429, #12511, #3300, #2416 ) ) ;
#8237 = FACE_OUTER_BOUND ( 'NONE', #11064, .T. ) ;
#8238 = CARTESIAN_POINT ( 'NONE',  ( 19.99999999999999645, 307.0000000000000568, 2.500000000000002220 ) ) ;
#8239 = CARTESIAN_POINT ( 'NONE',  ( -2.500000000000000000, 247.0000000000000284, -40.00000000000000000 ) ) ;
#8240 = CARTESIAN_POINT ( 'NONE',  ( -49.86468353124999453, 27.82187500034139305, -16.20201782572375393 ) ) ;
#8241 = EDGE_CURVE ( 'NONE', #9035, #9419, #15420, .T. ) ;
#8242 = CARTESIAN_POINT ( 'NONE',  ( -49.99999999999999289, 48.09999999999999432, 16.24598481164533226 ) ) ;
#8243 = CARTESIAN_POINT ( 'NONE',  ( 16.48898053797764973, 28.38332565970932819, 101.0000000000000000 ) ) ;
#8244 = CARTESIAN_POINT ( 'NONE',  ( -16.72075857324118786, 7.444561356925489370, 101.0000000000000000 ) ) ;
#8245 = FACE_OUTER_BOUND ( 'NONE', #622, .T. ) ;
#8246 = CARTESIAN_POINT ( 'NONE',  ( 9.289494224341416029, 8.863457290943287603, 102.0000000000000142 ) ) ;
#8247 = EDGE_CURVE ( 'NONE', #10886, #13613, #3847, .T. ) ;
#8248 = CARTESIAN_POINT ( 'NONE',  ( 49.99999999999999289, 35.10000000000000853, -16.24598481164532160 ) ) ;
#8249 = CARTESIAN_POINT ( 'NONE',  ( -49.86468353125000164, 23.85937500034139447, 0.000000000000000000 ) ) ;
#8250 = DIRECTION ( 'NONE',  ( 0.000000000000000000, 0.000000000000000000, -1.000000000000000000 ) ) ;
#8251 = ORIENTED_EDGE ( 'NONE', *, *, #2008, .F. ) ;
#8252 = ADVANCED_FACE ( 'NONE', ( #10119 ), #5226, .T. ) ;
#8253 = UNCERTAINTY_MEASURE_WITH_UNIT (LENGTH_MEASURE( 1.000000000000000082E-05 ), #9805, 'distance_accuracy_value', 'NONE');
#8254 = CARTESIAN_POINT ( 'NONE',  ( -40.34137639590981195, 30.05937500034139731, 29.30972558990012189 ) ) ;
#8255 = ORIENTED_EDGE ( 'NONE', *, *, #5509, .F. ) ;
#8256 = FACE_OUTER_BOUND ( 'NONE', #6363, .T. ) ;
#8257 = CARTESIAN_POINT ( 'NONE',  ( 49.86468353125001585, 40.75937500034138594, 16.20201782572375038 ) ) ;
#8258 = CARTESIAN_POINT ( 'NONE',  ( 29.34549410641285405, 282.0000000000000000, 12.17274705320883754 ) ) ;
#8259 =( BOUNDED_CURVE ( )  B_SPLINE_CURVE ( 2, ( #2217, #4830, #7152, #2310, #5983, #11052, #9885, #1970, #3312, #812, #5902, #4494, #15873 ),
 .UNSPECIFIED., .F., .T. ) 
 B_SPLINE_CURVE_WITH_KNOTS ( ( 3, 2, 2, 2, 2, 2, 3 ),
 ( 0.2166666666666666741, 0.2200000000000000011, 0.2266666666666666552, 0.2333333333333333370, 0.2399999999999999911, 0.2466666666666666730, 0.2500000000000000000 ),
 .UNSPECIFIED. ) 
 CURVE ( )  GEOMETRIC_REPRESENTATION_ITEM ( )  RATIONAL_B_SPLINE_CURVE ( ( 0.9755282581475768211, 0.9755282581475768211, 1.000000000000000000, 0.9510565162951535312, 1.000000000000000000, 0.9510565162951535312, 1.000000000000000000, 0.9510565162951535312, 1.000000000000000000, 0.9510565162951535312, 1.000000000000000000, 0.9755282581475768211, 0.9755282581475765991 ) ) 
 REPRESENTATION_ITEM ( '' )  );
#8260 = DIRECTION ( 'NONE',  ( 0.000000000000000000, 0.000000000000000000, -1.000000000000000000 ) ) ;
#8261 = CARTESIAN_POINT ( 'NONE',  ( 40.34137639590981195, 27.12187500034139731, -29.30972558990011834 ) ) ;
#8262 = CARTESIAN_POINT ( 'NONE',  ( 30.81806926056964002, 34.55937500034139731, 42.41743335407646498 ) ) ;
#8263 = CARTESIAN_POINT ( 'NONE',  ( -49.99999999999999289, 44.09999999999999432, 16.24598481164533226 ) ) ;
#8264 = CARTESIAN_POINT ( 'NONE',  ( -3.210462471511496205E-15, 29.42187500034139092, -52.43083105670540789 ) ) ;
#8265 = CARTESIAN_POINT ( 'NONE',  ( -49.99999999999999289, 43.90000000000000568, -16.24598481164531449 ) ) ;
#8266 = CARTESIAN_POINT ( 'NONE',  ( 30.81806926056964002, 44.55937500034139020, 42.41743335407647209 ) ) ;
#8267 = CARTESIAN_POINT ( 'NONE',  ( 30.81806926056962936, 41.22187500034139873, -42.41743335407647209 ) ) ;
#8268 = CARTESIAN_POINT ( 'NONE',  ( 15.45084971874737789, 48.60000000000000142, 47.55282581475767500 ) ) ;
#8269 = EDGE_CURVE ( 'NONE', #7797, #5335, #1544, .T. ) ;
#8270 = ORIENTED_EDGE ( 'NONE', *, *, #10483, .T. ) ;
#8271 = CARTESIAN_POINT ( 'NONE',  ( 49.86468353125001585, 48.75937500034140015, 16.20201782572375038 ) ) ;
#8272 = VERTEX_POINT ( 'NONE', #12692 ) ;
#8273 = ORIENTED_EDGE ( 'NONE', *, *, #6942, .F. ) ;
#8274 = CARTESIAN_POINT ( 'NONE',  ( -40.45084971874737079, 27.98125000068279888, 29.38926261462367151 ) ) ;
#8275 = VERTEX_POINT ( 'NONE', #4040 ) ;
#8276 = LINE ( 'NONE', #11936, #16083 ) ;
#8277 = CARTESIAN_POINT ( 'NONE',  ( -30.81806926056963292, 37.62187500034138310, -42.41743335407646498 ) ) ;
#8278 = CARTESIAN_POINT ( 'NONE',  ( 49.86468353125001585, 46.82187500034139305, 16.20201782572375038 ) ) ;
#8279 = CARTESIAN_POINT ( 'NONE',  ( -1.240322475938754499E-13, 40.28125000068280315, 50.00000000000000000 ) ) ;
#8280 = ITEM_DEFINED_TRANSFORMATION ( 'NONE', 'NONE', #14743,  #15812 ) ;
#8281 = CARTESIAN_POINT ( 'NONE',  ( 40.45084971874737789, 40.80000000000000426, 29.38926261462365375 ) ) ;
#8282 = CARTESIAN_POINT ( 'NONE',  ( 15.40903463028482356, 38.52187500034139589, 47.42413220539093999 ) ) ;
#8283 = CARTESIAN_POINT ( 'NONE',  ( 15.45084971874737789, 30.60000000000000142, 47.55282581475767500 ) ) ;
#8284 = ORIENTED_EDGE ( 'NONE', *, *, #3000, .F. ) ;
#8285 = CARTESIAN_POINT ( 'NONE',  ( 49.86468353125001585, 44.82187500034138594, 16.20201782572375038 ) ) ;
#8286 = EDGE_LOOP ( 'NONE', ( #4924, #4058 ) ) ;
#8287 = ORIENTED_EDGE ( 'NONE', *, *, #1358, .F. ) ;
#8288 = EDGE_CURVE ( 'NONE', #10597, #15517, #11372, .T. ) ;
#8289 = ORIENTED_EDGE ( 'NONE', *, *, #10208, .F. ) ;
#8290 = EDGE_CURVE ( 'NONE', #14428, #8817, #7263, .T. ) ;
#8291 = DIRECTION ( 'NONE',  ( 1.000000000000000000, -0.000000000000000000, -0.000000000000000000 ) ) ;
#8292 = CARTESIAN_POINT ( 'NONE',  ( 7.594208199954109127E-15, 52.26146722824297797, -62.01141590572476758 ) ) ;
#8293 = CARTESIAN_POINT ( 'NONE',  ( -30.90169943749473802, 20.30000000000000426, 42.53254041760200721 ) ) ;
#8294 = CARTESIAN_POINT ( 'NONE',  ( -40.34137639590981195, 40.05937500034140442, 29.30972558990012189 ) ) ;
#8295 = CARTESIAN_POINT ( 'NONE',  ( 24.78626291527397285, 40.00000000000000711, 5.650101528493621572 ) ) ;
#8296 = CARTESIAN_POINT ( 'NONE',  ( -2.500000000000000000, 247.0000000000000284, 47.99999999999999289 ) ) ;
#8297 = CARTESIAN_POINT ( 'NONE',  ( -40.45084971874737789, 33.58125000068280031, -29.38926261462365730 ) ) ;
#8298 = PRESENTATION_STYLE_ASSIGNMENT (( #12371 ) ) ;
#8299 = PLANE ( 'NONE',  #16303 ) ;
#8300 =( BOUNDED_CURVE ( )  B_SPLINE_CURVE ( 2, ( #5596, #6922, #5432, #7082, #13303, #14540, #15885, #6997, #13229, #497, #10658, #9249, #3168 ),
 .UNSPECIFIED., .F., .F. ) 
 B_SPLINE_CURVE_WITH_KNOTS ( ( 3, 2, 2, 2, 2, 2, 3 ),
 ( 0.05000000000000000278, 0.05333333333333333676, 0.05999999999999999778, 0.06666666666666666574, 0.07333333333333333370, 0.08000000000000000167, 0.08333333333333334259 ),
 .UNSPECIFIED. ) 
 CURVE ( )  GEOMETRIC_REPRESENTATION_ITEM ( )  RATIONAL_B_SPLINE_CURVE ( ( 0.9755282581475768211, 0.9755282581475768211, 1.000000000000000000, 0.9510565162951535312, 1.000000000000000000, 0.9510565162951535312, 1.000000000000000000, 0.9510565162951535312, 1.000000000000000000, 0.9510565162951535312, 1.000000000000000000, 0.9755282581475767101, 0.9755282581475768211 ) ) 
 REPRESENTATION_ITEM ( '' )  );
#8301 = CARTESIAN_POINT ( 'NONE',  ( -49.99999999999999289, 46.09999999999999432, 16.24598481164533226 ) ) ;
#8302 = AXIS2_PLACEMENT_3D ( 'NONE', #6316, #890, #2471 ) ;
#8303 = CARTESIAN_POINT ( 'NONE',  ( 40.45084971874737079, 41.20000000000000284, -29.38926261462366440 ) ) ;
#8304 = DIRECTION ( 'NONE',  ( 0.8090169943749504489, -0.5877852522924689183, 0.000000000000000000 ) ) ;
#8305 = EDGE_LOOP ( 'NONE', ( #2146, #162, #2150, #10968 ) ) ;
#8306 = CARTESIAN_POINT ( 'NONE',  ( 15.40903463028481113, 33.25937500034140015, -47.42413220539094709 ) ) ;
#8307 = ORIENTED_EDGE ( 'NONE', *, *, #1657, .F. ) ;
#8308 = EDGE_LOOP ( 'NONE', ( #9529, #14514, #8843, #9809 ) ) ;
#8309 = EDGE_LOOP ( 'NONE', ( #8513, #10464, #8841, #2626 ) ) ;
#8310 = CARTESIAN_POINT ( 'NONE',  ( 40.45084971874737789, 46.58125000068280031, 29.38926261462365375 ) ) ;
#8311 = CARTESIAN_POINT ( 'NONE',  ( 0.000000000000000000, 20.00000000000000355, 0.000000000000000000 ) ) ;
#8313 = ORIENTED_EDGE ( 'NONE', *, *, #8383, .F. ) ;
#8312 = CIRCLE ( 'NONE', #1131, 60.00000000000000711 ) ;
#8314 = CARTESIAN_POINT ( 'NONE',  ( -15.45084971874736368, 38.40000000000000568, 47.55282581475768211 ) ) ;
#8315 = DIRECTION ( 'NONE',  ( 0.7431448254773955764, -0.6691306063588567943, 0.000000000000000000 ) ) ;
#8316 = DIRECTION ( 'NONE',  ( -1.000000000000000000, 0.000000000000000000, -2.602085213965210149E-16 ) ) ;
#8317 = CARTESIAN_POINT ( 'NONE',  ( 43.87482193696061472, 267.0000000000000000, 10.00000000000000178 ) ) ;
#8318 = PLANE ( 'NONE',  #2364 ) ;
#8319 = CARTESIAN_POINT ( 'NONE',  ( -49.99999999999999289, 31.89999999999999858, -16.24598481164531449 ) ) ;
#8320 = CARTESIAN_POINT ( 'NONE',  ( 50.00000000000000711, 36.68125000068280173, 16.24598481164530739 ) ) ;
#8321 = CARTESIAN_POINT ( 'NONE',  ( 0.000000000000000000, 193.4213562373095385, -50.00000000000000000 ) ) ;
#8322 = CARTESIAN_POINT ( 'NONE',  ( -30.81806926056962226, 22.22187500034139163, 42.41743335407647209 ) ) ;
#8323 = DIRECTION ( 'NONE',  ( 0.000000000000000000, 0.000000000000000000, -1.000000000000000000 ) ) ;
#8324 = CARTESIAN_POINT ( 'NONE',  ( 15.45084971874737789, 36.60000000000000142, 47.55282581475767500 ) ) ;
#8325 = CARTESIAN_POINT ( 'NONE',  ( 30.81806926056962936, 25.15937500034139518, -42.41743335407647209 ) ) ;
#8326 = CIRCLE ( 'NONE', #4353, 5.000000000000000000 ) ;
#8327 = CARTESIAN_POINT ( 'NONE',  ( 15.40903463028481113, 49.25937500034139305, -47.42413220539094709 ) ) ;
#8328 = ORIENTED_EDGE ( 'NONE', *, *, #12849, .F. ) ;
#8329 = ADVANCED_FACE ( 'NONE', ( #14087 ), #9032, .T. ) ;
#8330 = CARTESIAN_POINT ( 'NONE',  ( -1.688807283342573573, 101.8522485078275253, 9.657683769731223222 ) ) ;
#8331 = ORIENTED_EDGE ( 'NONE', *, *, #16259, .F. ) ;
#8332 = LINE ( 'NONE', #13396, #11582 ) ;
#8333 = CARTESIAN_POINT ( 'NONE',  ( -49.86468353124999453, 41.75937500034139305, -16.20201782572375393 ) ) ;
#8334 = CARTESIAN_POINT ( 'NONE',  ( 19.99999999999999645, 307.0000000000000568, -2.499999999999999556 ) ) ;
#8335 = CARTESIAN_POINT ( 'NONE',  ( 0.000000000000000000, 193.4213562373095385, -50.00000000000000000 ) ) ;
#8336 = EDGE_CURVE ( 'NONE', #8062, #10751, #12605, .T. ) ;
#8337 = AXIS2_PLACEMENT_3D ( 'NONE', #14201, #7896, #12971 ) ;
#8338 = CARTESIAN_POINT ( 'NONE',  ( 0.000000000000000000, 22.50000000000000000, 102.0000000000000142 ) ) ;
#8339 = CARTESIAN_POINT ( 'NONE',  ( 40.34137639590981905, 30.72187500034139518, 29.30972558990010768 ) ) ;
#8340 = CARTESIAN_POINT ( 'NONE',  ( -15.40903463028481646, 31.45937500034139944, -47.42413220539093999 ) ) ;
#8341 = FACE_OUTER_BOUND ( 'NONE', #567, .T. ) ;
#8342 = CARTESIAN_POINT ( 'NONE',  ( 15.40903463028482356, 32.52187500034139589, 47.42413220539093999 ) ) ;
#8343 = EDGE_CURVE ( 'NONE', #16281, #332, #7859, .T. ) ;
#8344 = CARTESIAN_POINT ( 'NONE',  ( -15.40903463028480580, 46.25937500034140015, 47.42413220539094709 ) ) ;
#8345 = CARTESIAN_POINT ( 'NONE',  ( -49.86468353124999453, 35.82187500034139305, -16.20201782572375393 ) ) ;
#8346 = CARTESIAN_POINT ( 'NONE',  ( 49.86468353125000164, 20.92187500034139802, -6.106662507704105588E-15 ) ) ;
#8347 = VERTEX_POINT ( 'NONE', #12940 ) ;
#8348 = CIRCLE ( 'NONE', #3303, 79.49773270518484480 ) ;
#8349 = EDGE_CURVE ( 'NONE', #12433, #16149, #4679, .T. ) ;
#8350 = CARTESIAN_POINT ( 'NONE',  ( -40.34137639590981195, 40.05937500034140442, 29.30972558990012189 ) ) ;
#8351 = ORIENTED_EDGE ( 'NONE', *, *, #7340, .T. ) ;
#8352 = CARTESIAN_POINT ( 'NONE',  ( 30.90169943749474157, 33.08125000068279320, -42.53254041760200721 ) ) ;
#8353 = ORIENTED_EDGE ( 'NONE', *, *, #11096, .T. ) ;
#8354 = CARTESIAN_POINT ( 'NONE',  ( -30.90169943749473447, 36.29999999999999716, 42.53254041760200721 ) ) ;
#8355 = CARTESIAN_POINT ( 'NONE',  ( 15.40903463028481113, 39.32187500034140015, -47.42413220539094709 ) ) ;
#8356 = CARTESIAN_POINT ( 'NONE',  ( -40.34137639590981905, 49.72187500034139873, -29.30972558990011478 ) ) ;
#8357 = DIRECTION ( 'NONE',  ( -0.9510565162951503115, -0.3090169943749574988, 0.000000000000000000 ) ) ;
#8358 = CIRCLE ( 'NONE', #1182, 17.50000000000000000 ) ;
#8359 = CARTESIAN_POINT ( 'NONE',  ( 40.34137639590981905, 24.72187500034139873, 29.30972558990010768 ) ) ;
#8360 = CARTESIAN_POINT ( 'NONE',  ( -49.99999999999999289, 36.10000000000000853, 16.24598481164533226 ) ) ;
#8361 = CARTESIAN_POINT ( 'NONE',  ( -49.86468353124999453, 40.02187500034140299, 16.20201782572377525 ) ) ;
#8362 = DIRECTION ( 'NONE',  ( 0.000000000000000000, -1.000000000000000000, -0.000000000000000000 ) ) ;
#8363 = ORIENTED_EDGE ( 'NONE', *, *, #7178, .F. ) ;
#8364 = EDGE_CURVE ( 'NONE', #14778, #10814, #12530, .T. ) ;
#8365 = CARTESIAN_POINT ( 'NONE',  ( 30.81806926056962936, 39.22187500034139873, -42.41743335407647209 ) ) ;
#8366 = ORIENTED_EDGE ( 'NONE', *, *, #2468, .F. ) ;
#8367 = ORIENTED_EDGE ( 'NONE', *, *, #10730, .T. ) ;
#8368 = CIRCLE ( 'NONE', #5203, 16.50000000000000711 ) ;
#8369 = VERTEX_POINT ( 'NONE', #10286 ) ;
#8370 = CARTESIAN_POINT ( 'NONE',  ( 8.446640517145639571E-15, 48.49999999999999289, 50.00000000000000000 ) ) ;
#8371 = DIRECTION ( 'NONE',  ( 0.000000000000000000, -0.7890408728378107694, -0.6143407043256581268 ) ) ;
#8372 = CARTESIAN_POINT ( 'NONE',  ( 50.00000000000000711, 36.68125000068280173, 16.24598481164530739 ) ) ;
#8373 = CARTESIAN_POINT ( 'NONE',  ( 30.81806926056964002, 40.55937500034139731, 42.41743335407647209 ) ) ;
#8374 = CARTESIAN_POINT ( 'NONE',  ( 30.81806926056962936, 47.15937500034139163, -42.41743335407646498 ) ) ;
#8375 = CARTESIAN_POINT ( 'NONE',  ( -15.45084971874736368, 30.40000000000000213, 47.55282581475768211 ) ) ;
#8376 = LINE ( 'NONE', #16198, #16370 ) ;
#8377 = CONICAL_SURFACE ( 'NONE', #1201, 16.50000000000000711, 0.7853981633974447263 ) ;
#8379 = LINE ( 'NONE', #5898, #6485 ) ;
#8378 = VECTOR ( 'NONE', #12027, 1000.000000000000114 ) ;
#8380 = CARTESIAN_POINT ( 'NONE',  ( -30.90169943749473447, 36.08125000068279320, 42.53254041760200721 ) ) ;
#8381 = CIRCLE ( 'NONE', #9723, 2.000000000000001776 ) ;
#8382 = CARTESIAN_POINT ( 'NONE',  ( 1.486087262401875941, 13.10364194761998213, 102.0000000000000142 ) ) ;
#8383 = EDGE_CURVE ( 'NONE', #5335, #6657, #7621, .T. ) ;
#8384 = CARTESIAN_POINT ( 'NONE',  ( 0.000000000000000000, 28.00000000000000355, 0.000000000000000000 ) ) ;
#8385 = PRODUCT_DEFINITION_FORMATION_WITH_SPECIFIED_SOURCE ( 'ANY', '', #1877, .NOT_KNOWN. ) ;
#8386 = VERTEX_POINT ( 'NONE', #1454 ) ;
#8387 = CARTESIAN_POINT ( 'NONE',  ( -49.86468353124999453, 33.75937500034140015, -16.20201782572375393 ) ) ;
#8388 = ORIENTED_EDGE ( 'NONE', *, *, #10990, .F. ) ;
#8389 = ORIENTED_EDGE ( 'NONE', *, *, #1857, .F. ) ;
#8390 = ORIENTED_EDGE ( 'NONE', *, *, #1427, .T. ) ;
#8391 = CARTESIAN_POINT ( 'NONE',  ( -50.00000000000000000, 45.78125000068279604, 0.000000000000000000 ) ) ;
#8392 = AXIS2_PLACEMENT_3D ( 'NONE', #8338, #927, #12245 ) ;
#8393 = AXIS2_PLACEMENT_3D ( 'NONE', #5314, #9204, #2881 ) ;
#8394 = CARTESIAN_POINT ( 'NONE',  ( 49.99999999999999289, 47.10000000000000142, -16.24598481164532160 ) ) ;
#8395 = VECTOR ( 'NONE', #958, 1000.000000000000000 ) ;
#8396 = ORIENTED_EDGE ( 'NONE', *, *, #12831, .F. ) ;
#8397 = CARTESIAN_POINT ( 'NONE',  ( 0.000000000000000000, 22.50000000000000000, 101.0000000000000000 ) ) ;
#8398 = CARTESIAN_POINT ( 'NONE',  ( 0.000000000000000000, 193.4213562373095385, 0.000000000000000000 ) ) ;
#8399 = CARTESIAN_POINT ( 'NONE',  ( -3.111920190527341144E-15, 45.28125000068279604, -50.00000000000000000 ) ) ;
#8400 = LINE ( 'NONE', #7409, #2002 ) ;
#8401 = DIRECTION ( 'NONE',  ( -0.000000000000000000, -0.000000000000000000, 1.000000000000000000 ) ) ;
#8402 = DIRECTION ( 'NONE',  ( 1.000000000000000000, -0.000000000000000000, -0.000000000000000000 ) ) ;
#8403 =( BOUNDED_CURVE ( )  B_SPLINE_CURVE ( 3, ( #9906, #14960, #3333, #6094 ),
 .UNSPECIFIED., .F., .F. ) 
 B_SPLINE_CURVE_WITH_KNOTS ( ( 4, 4 ),
 ( 1.570796326794897002, 3.141592653589793116 ),
 .UNSPECIFIED. ) 
 CURVE ( )  GEOMETRIC_REPRESENTATION_ITEM ( )  RATIONAL_B_SPLINE_CURVE ( ( 1.000000000000000000, 0.8047378541243650485, 0.8047378541243650485, 1.000000000000000000 ) ) 
 REPRESENTATION_ITEM ( '' )  );
#8404 = CARTESIAN_POINT ( 'NONE',  ( -40.45084971874737789, 31.80000000000000071, -29.38926261462365730 ) ) ;
#8405 =( LENGTH_UNIT ( ) NAMED_UNIT ( * ) SI_UNIT ( .MILLI., .METRE. ) );
#8406 = CARTESIAN_POINT ( 'NONE',  ( -46.13167797950591620, 20.00000000000000355, 18.93026546213454608 ) ) ;
#8407 = CARTESIAN_POINT ( 'NONE',  ( -30.81806926056963292, 23.62187500034139731, -42.41743335407646498 ) ) ;
#8408 = FACE_OUTER_BOUND ( 'NONE', #10218, .T. ) ;
#8409 = AXIS2_PLACEMENT_3D ( 'NONE', #10251, #2430, #2511 ) ;
#8410 = CARTESIAN_POINT ( 'NONE',  ( -3.219174618344376363E-15, 25.50000000000000355, -52.57311121191334990 ) ) ;
#8411 = CARTESIAN_POINT ( 'NONE',  ( 49.86468353125001585, 24.75937500034140015, 16.20201782572375038 ) ) ;
#8412 = VECTOR ( 'NONE', #5353, 1000.000000000000000 ) ;
#8413 = CARTESIAN_POINT ( 'NONE',  ( 40.34137639590981905, 48.65937500034139873, 29.30972558990010768 ) ) ;
#8414 = ORIENTED_EDGE ( 'NONE', *, *, #12611, .T. ) ;
#8415 = PRODUCT_DEFINITION_CONTEXT ( 'detailed design', #10053, 'design' ) ;
#8416 = CARTESIAN_POINT ( 'NONE',  ( 30.81806926056964002, 26.55937500034139376, 42.41743335407646498 ) ) ;
#8417 = EDGE_LOOP ( 'NONE', ( #16010, #5030, #2787, #15325 ) ) ;
#8418 = CARTESIAN_POINT ( 'NONE',  ( 30.90169943749475223, 48.69999999999999574, 42.53254041760199300 ) ) ;
#8419 = CARTESIAN_POINT ( 'NONE',  ( 30.81806926056962936, 33.15937500034139873, -42.41743335407647209 ) ) ;
#8420 = EDGE_CURVE ( 'NONE', #13132, #102, #9241, .T. ) ;
#8421 = AXIS2_PLACEMENT_3D ( 'NONE', #6755, #4407, #1736 ) ;
#8422 = ADVANCED_FACE ( 'NONE', ( #1939 ), #14573, .T. ) ;
#8423 = CARTESIAN_POINT ( 'NONE',  ( 49.99999999999999289, 40.88125000068279746, -16.24598481164532160 ) ) ;
#8424 = CARTESIAN_POINT ( 'NONE',  ( 30.90169943749475223, 34.70000000000000284, 42.53254041760199300 ) ) ;
#8425 = CIRCLE ( 'NONE', #12137, 82.49773270518484480 ) ;
#8426 = CARTESIAN_POINT ( 'NONE',  ( 0.000000000000000000, 193.4213562373095385, 0.000000000000000000 ) ) ;
#8427 = CARTESIAN_POINT ( 'NONE',  ( -30.81806926056962226, 30.22187500034139518, 42.41743335407647919 ) ) ;
#8428 = CARTESIAN_POINT ( 'NONE',  ( -30.81806926056962226, 30.15937500034139163, 42.41743335407647209 ) ) ;
#8429 = CARTESIAN_POINT ( 'NONE',  ( -49.86468353125000164, 31.92187500034139447, 0.000000000000000000 ) ) ;
#8430 = CARTESIAN_POINT ( 'NONE',  ( -3.111920190527341144E-15, 29.50000000000000000, -50.00000000000000000 ) ) ;
#8431 = CARTESIAN_POINT ( 'NONE',  ( 30.81806926056962936, 43.15937500034140584, -42.41743335407647209 ) ) ;
#8432 = CARTESIAN_POINT ( 'NONE',  ( 40.34137639590981905, 34.72187500034139873, 29.30972558990010768 ) ) ;
#8433 = CARTESIAN_POINT ( 'NONE',  ( -50.00000000000000000, 50.00000000000000000, 0.000000000000000000 ) ) ;
#8434 = EDGE_CURVE ( 'NONE', #9682, #7797, #15671, .T. ) ;
#8435 = VERTEX_POINT ( 'NONE', #9358 ) ;
#8436 = CARTESIAN_POINT ( 'NONE',  ( -30.81806926056963292, 39.55937500034140442, -42.41743335407646498 ) ) ;
#8437 = VERTEX_POINT ( 'NONE', #14408 ) ;
#8438 = CARTESIAN_POINT ( 'NONE',  ( 15.45084971874737789, 22.38125000068280102, 47.55282581475767500 ) ) ;
#8439 = VERTEX_POINT ( 'NONE', #3197 ) ;
#8440 = FACE_OUTER_BOUND ( 'NONE', #15710, .T. ) ;
#8441 = CARTESIAN_POINT ( 'NONE',  ( 49.86468353124999453, 41.02187500034139589, -16.20201782572376104 ) ) ;
#8442 = CONICAL_SURFACE ( 'NONE', #2606, 16.50000000000000711, 0.7853981633974447263 ) ;
#8443 = CARTESIAN_POINT ( 'NONE',  ( 49.86468353125001585, 20.75937500034140015, 16.20201782572375038 ) ) ;
#8444 = LINE ( 'NONE', #12264, #10765 ) ;
#8445 = EDGE_CURVE ( 'NONE', #7884, #1138, #12439, .T. ) ;
#8446 = CARTESIAN_POINT ( 'NONE',  ( 15.40903463028481113, 23.32187500034139660, -47.42413220539094709 ) ) ;
#8447 = CARTESIAN_POINT ( 'NONE',  ( 40.45084971874737789, 36.58125000068280031, 29.38926261462365375 ) ) ;
#8448 = CARTESIAN_POINT ( 'NONE',  ( 30.90169943749475578, 38.70000000000000284, 42.53254041760200010 ) ) ;
#8449 = CARTESIAN_POINT ( 'NONE',  ( -15.40903463028481646, 39.52187500034139589, -47.42413220539093999 ) ) ;
#8450 = DIRECTION ( 'NONE',  ( 0.3420201433256697121, 0.6644630243886755494, -0.6644630243886733290 ) ) ;
#8451 = EDGE_LOOP ( 'NONE', ( #9456, #15363, #14353, #2122 ) ) ;
#8452 = CARTESIAN_POINT ( 'NONE',  ( 40.34137639590981905, 42.72187500034139873, 29.30972558990010768 ) ) ;
#8453 = EDGE_CURVE ( 'NONE', #9685, #1121, #9588, .T. ) ;
#8454 = CARTESIAN_POINT ( 'NONE',  ( -7.919222016226838967, 44.22999571913595673, 49.99999999999999289 ) ) ;
#8455 = EDGE_LOOP ( 'NONE', ( #6017, #10057 ) ) ;
#8456 = ORIENTED_EDGE ( 'NONE', *, *, #1250, .F. ) ;
#8457 = EDGE_CURVE ( 'NONE', #12470, #7298, #14745, .T. ) ;
#8458 = ORIENTED_EDGE ( 'NONE', *, *, #14127, .T. ) ;
#8459 = DIRECTION ( 'NONE',  ( 6.938893903907231459E-18, -1.000000000000000000, -5.551115123125782702E-17 ) ) ;
#8460 = DIRECTION ( 'NONE',  ( -0.000000000000000000, -1.000000000000000000, -0.000000000000000000 ) ) ;
#8461 = CARTESIAN_POINT ( 'NONE',  ( 1.022488062601840571E-14, 49.28125000068280315, -50.00000000000000000 ) ) ;
#8462 = CARTESIAN_POINT ( 'NONE',  ( 0.000000000000000000, 20.00000000000000355, 0.000000000000000000 ) ) ;
#8463 = CARTESIAN_POINT ( 'NONE',  ( 40.34137639590981905, 40.65937500034139873, 29.30972558990010768 ) ) ;
#8464 = CARTESIAN_POINT ( 'NONE',  ( 40.34137639590981905, 46.65937500034139873, 29.30972558990010768 ) ) ;
#8465 = LINE ( 'NONE', #14601, #1570 ) ;
#8466 = CARTESIAN_POINT ( 'NONE',  ( -7.580410092413979228, 101.3368000520362813, -5.000000000000000000 ) ) ;
#8467 = CARTESIAN_POINT ( 'NONE',  ( 6.251299836021209089, 37.76994598419266680, 102.0000000000000142 ) ) ;
#8468 = PLANE ( 'NONE',  #11871 ) ;
#8469 = CARTESIAN_POINT ( 'NONE',  ( 7.919222016226758143, 40.55125428154685352, 50.00000000000000711 ) ) ;
#8470 = PLANE ( 'NONE',  #2718 ) ;
#8471 = EDGE_LOOP ( 'NONE', ( #7233, #1028, #7819, #3135, #858, #4571, #15153, #7801, #14636, #16450, #1620, #14149, #644 ) ) ;
#8472 = CARTESIAN_POINT ( 'NONE',  ( 40.34137639590981905, 30.65937500034139518, 29.30972558990010768 ) ) ;
#8473 = VERTEX_POINT ( 'NONE', #4602 ) ;
#8474 = VERTEX_POINT ( 'NONE', #14801 ) ;
#8475 = ORIENTED_EDGE ( 'NONE', *, *, #5533, .F. ) ;
#8476 = EDGE_CURVE ( 'NONE', #7924, #960, #6734, .T. ) ;
#8477 = CARTESIAN_POINT ( 'NONE',  ( -30.90169943749474868, 41.48125000068278467, -42.53254041760200721 ) ) ;
#8478 = LINE ( 'NONE', #2230, #9162 ) ;
#8479 = ORIENTED_EDGE ( 'NONE', *, *, #10513, .F. ) ;
#8480 = LINE ( 'NONE', #9819, #6233 ) ;
#8481 = CARTESIAN_POINT ( 'NONE',  ( 0.000000000000000000, 20.00000000000000355, 50.00000000000000000 ) ) ;
#8482 = CARTESIAN_POINT ( 'NONE',  ( -15.45084971874736368, 20.40000000000000213, 47.55282581475768211 ) ) ;
#8483 = CYLINDRICAL_SURFACE ( 'NONE', #4146, 17.50000000000000000 ) ;
#8484 = DIRECTION ( 'NONE',  ( 1.734723475976807094E-17, -0.000000000000000000, 1.000000000000000000 ) ) ;
#8485 = FACE_OUTER_BOUND ( 'NONE', #3295, .T. ) ;
#8486 = CARTESIAN_POINT ( 'NONE',  ( 49.99999999999999289, 39.10000000000000142, -16.24598481164532160 ) ) ;
#8487 = CARTESIAN_POINT ( 'NONE',  ( 7.513064459987437071E-14, 42.50000000000000000, 50.00000000000000000 ) ) ;
#8488 = CARTESIAN_POINT ( 'NONE',  ( 9.657683769731171708, 93.19872860642226442, 1.198728606422249987 ) ) ;
#8489 = CARTESIAN_POINT ( 'NONE',  ( 5.755839955992560641E-15, 51.99999999999999289, 47.00000000000000000 ) ) ;
#8490 = VECTOR ( 'NONE', #3141, 1000.000000000000000 ) ;
#8491 = CARTESIAN_POINT ( 'NONE',  ( 49.99999999999999289, 29.10000000000000142, -16.24598481164532160 ) ) ;
#8492 = CARTESIAN_POINT ( 'NONE',  ( -30.81806926056963292, 27.55937500034139376, -42.41743335407647209 ) ) ;
#8493 = CARTESIAN_POINT ( 'NONE',  ( -50.00000000000000000, 44.00000000000000711, 0.000000000000000000 ) ) ;
#8494 = CARTESIAN_POINT ( 'NONE',  ( -49.99999999999999289, 30.10000000000000497, 16.24598481164533226 ) ) ;
#8495 = ORIENTED_EDGE ( 'NONE', *, *, #6633, .F. ) ;
#8496 = CARTESIAN_POINT ( 'NONE',  ( 40.45084971874737789, 44.79999999999999716, 29.38926261462365375 ) ) ;
#8497 = ORIENTED_EDGE ( 'NONE', *, *, #4317, .T. ) ;
#8498 = DIRECTION ( 'NONE',  ( -0.000000000000000000, -1.000000000000000000, -0.000000000000000000 ) ) ;
#8500 = CARTESIAN_POINT ( 'NONE',  ( 49.86468353124999453, 32.95937500034138168, -16.20201782572376459 ) ) ;
#8499 =( BOUNDED_CURVE ( )  B_SPLINE_CURVE ( 3, ( #12354, #11127, #16187, #12447 ),
 .UNSPECIFIED., .F., .F. ) 
 B_SPLINE_CURVE_WITH_KNOTS ( ( 4, 4 ),
 ( 0.000000000000000000, 1.570796326794896336 ),
 .UNSPECIFIED. ) 
 CURVE ( )  GEOMETRIC_REPRESENTATION_ITEM ( )  RATIONAL_B_SPLINE_CURVE ( ( 1.000000000000000000, 0.8047378541243650485, 0.8047378541243650485, 1.000000000000000000 ) ) 
 REPRESENTATION_ITEM ( '' )  );
#8501 = LINE ( 'NONE', #4865, #4160 ) ;
#8502 = CARTESIAN_POINT ( 'NONE',  ( 5.000000000000000000, 107.2206331336081462, 16.63484669598117094 ) ) ;
#8503 = CARTESIAN_POINT ( 'NONE',  ( 7.919222016226822092, 28.33250428222963890, 49.99999999999999289 ) ) ;
#8504 = DIRECTION ( 'NONE',  ( 2.312964634635742464E-16, 0.000000000000000000, -1.000000000000000000 ) ) ;
#8505 = CARTESIAN_POINT ( 'NONE',  ( -40.34137639590981195, 30.12187500034139731, 29.30972558990012189 ) ) ;
#8506 = CARTESIAN_POINT ( 'NONE',  ( -49.86468353124999453, 31.95937500034139944, 16.20201782572377169 ) ) ;
#8507 = CARTESIAN_POINT ( 'NONE',  ( 1.022488062601840571E-14, 49.50000000000000711, -50.00000000000000000 ) ) ;
#8508 = CARTESIAN_POINT ( 'NONE',  ( 49.86468353125000164, 28.92187500034139802, -6.106662507704105588E-15 ) ) ;
#8509 = CARTESIAN_POINT ( 'NONE',  ( 0.000000000000000000, 0.000000000000000000, 0.000000000000000000 ) ) ;
#8510 = CARTESIAN_POINT ( 'NONE',  ( -15.40903463028480580, 44.25937500034140015, 47.42413220539094709 ) ) ;
#8511 = CARTESIAN_POINT ( 'NONE',  ( -49.86468353125000164, 37.92187500034140157, 0.000000000000000000 ) ) ;
#8512 = CARTESIAN_POINT ( 'NONE',  ( 40.34137639590981195, 21.12187500034139376, -29.30972558990011834 ) ) ;
#8513 = ORIENTED_EDGE ( 'NONE', *, *, #4074, .T. ) ;
#8514 = CARTESIAN_POINT ( 'NONE',  ( -30.81806926056963292, 43.55937500034139731, -42.41743335407646498 ) ) ;
#8515 = VERTEX_POINT ( 'NONE', #12317 ) ;
#8516 = CARTESIAN_POINT ( 'NONE',  ( -30.90169943749474868, 25.48125000068279888, -42.53254041760200721 ) ) ;
#8517 = ORIENTED_EDGE ( 'NONE', *, *, #5866, .T. ) ;
#8518 = CARTESIAN_POINT ( 'NONE',  ( 0.000000000000000000, 267.0000000000000000, -45.00000000000000711 ) ) ;
#8519 = CARTESIAN_POINT ( 'NONE',  ( 9.631387414534489405E-15, 38.42187500034139447, 52.43083105670540789 ) ) ;
#8520 = CARTESIAN_POINT ( 'NONE',  ( -15.40903463028481646, 49.52187500034140299, -47.42413220539093999 ) ) ;
#8521 = CARTESIAN_POINT ( 'NONE',  ( 49.86468353124999453, 27.02187500034139589, -16.20201782572376459 ) ) ;
#8522 = CARTESIAN_POINT ( 'NONE',  ( -30.90169943749473802, 36.08125000068280031, 42.53254041760200721 ) ) ;
#8523 = CARTESIAN_POINT ( 'NONE',  ( -15.40903463028480580, 42.32187500034139305, 47.42413220539094709 ) ) ;
#8524 = CARTESIAN_POINT ( 'NONE',  ( -25.56848793686307175, 282.5058351977235134, -10.28424396843205457 ) ) ;
#8525 = VERTEX_POINT ( 'NONE', #7346 ) ;
#8526 = CARTESIAN_POINT ( 'NONE',  ( -40.34137639590981905, 37.72187500034139873, -29.30972558990011478 ) ) ;
#8527 = EDGE_LOOP ( 'NONE', ( #8819, #10948, #13140, #6136, #12564, #5, #13580, #8953, #10722, #6280, #10791, #12435, #4799, #10025, #229, #14464, #10812, #13616, #12526, #14842 ) ) ;
#8528 = ORIENTED_EDGE ( 'NONE', *, *, #1725, .F. ) ;
#8529 = EDGE_CURVE ( 'NONE', #2458, #3153, #14970, .T. ) ;
#8530 = ORIENTED_EDGE ( 'NONE', *, *, #6497, .F. ) ;
#8531 = CARTESIAN_POINT ( 'NONE',  ( -7.919222016226752814, 39.33250428222963535, -50.00000000000000711 ) ) ;
#8532 = DIRECTION ( 'NONE',  ( -1.000000000000000000, 0.000000000000000000, 0.000000000000000000 ) ) ;
#8533 = CARTESIAN_POINT ( 'NONE',  ( -9.395693774364753281, 21.00971865127312199, 102.0000000000000142 ) ) ;
#8534 = CYLINDRICAL_SURFACE ( 'NONE', #5556, 10.00000000000000000 ) ;
#8535 = CARTESIAN_POINT ( 'NONE',  ( -15.40903463028481646, 35.45937500034139589, -47.42413220539093999 ) ) ;
#8536 = DIRECTION ( 'NONE',  ( 0.4999999999999916178, 0.000000000000000000, -0.8660254037844433705 ) ) ;
#8537 = CARTESIAN_POINT ( 'NONE',  ( -15.45084971874737256, 29.60000000000000142, -47.55282581475767500 ) ) ;
#8538 = EDGE_CURVE ( 'NONE', #11555, #10428, #1154, .T. ) ;
#8539 = EDGE_CURVE ( 'NONE', #15190, #1407, #4658, .T. ) ;
#8540 = DIRECTION ( 'NONE',  ( 0.000000000000000000, 0.000000000000000000, -1.000000000000000000 ) ) ;
#8541 = DIRECTION ( 'NONE',  ( 1.000000000000000000, 0.000000000000000000, -0.000000000000000000 ) ) ;
#8542 = CARTESIAN_POINT ( 'NONE',  ( 40.45084971874737079, 37.20000000000000284, -29.38926261462366440 ) ) ;
#8543 = CARTESIAN_POINT ( 'NONE',  ( -49.99999999999999289, 41.90000000000000568, -16.24598481164531449 ) ) ;
#8544 = EDGE_LOOP ( 'NONE', ( #6340, #5718, #11012, #2720 ) ) ;
#8545 = CARTESIAN_POINT ( 'NONE',  ( 15.40903463028481113, 27.25937500034139660, -47.42413220539094709 ) ) ;
#8546 = ORIENTED_EDGE ( 'NONE', *, *, #11726, .T. ) ;
#8547 = ORIENTED_EDGE ( 'NONE', *, *, #4107, .T. ) ;
#8548 = ORIENTED_EDGE ( 'NONE', *, *, #7525, .T. ) ;
#8549 = CARTESIAN_POINT ( 'NONE',  ( -40.45084971874737079, 45.98125000068279888, 29.38926261462367151 ) ) ;
#8550 = CYLINDRICAL_SURFACE ( 'NONE', #1504, 50.00000000000000000 ) ;
#8551 = ORIENTED_EDGE ( 'NONE', *, *, #14343, .T. ) ;
#8552 = CARTESIAN_POINT ( 'NONE',  ( 5.510910596163089556E-15, 217.0000000000000284, -45.00000000000000000 ) ) ;
#8553 = SURFACE_SIDE_STYLE ('',( #13302 ) ) ;
#8554 = CARTESIAN_POINT ( 'NONE',  ( -11.62776035141319397, 9.371681691055611552, 97.66124091237762173 ) ) ;
#8555 = CARTESIAN_POINT ( 'NONE',  ( 0.000000000000000000, 0.000000000000000000, 100.0000000000000000 ) ) ;
#8556 = CARTESIAN_POINT ( 'NONE',  ( 1.106078086759636654E-14, 273.6527036446661896, -89.78914894885470233 ) ) ;
#8557 = DIRECTION ( 'NONE',  ( 0.000000000000000000, 0.000000000000000000, -1.000000000000000000 ) ) ;
#8559 = CARTESIAN_POINT ( 'NONE',  ( 40.45084971874737079, 39.19999999999999574, -29.38926261462366440 ) ) ;
#8558 = VECTOR ( 'NONE', #2218, 1000.000000000000000 ) ;
#8560 = DIRECTION ( 'NONE',  ( 1.000000000000000000, 0.000000000000000000, 0.000000000000000000 ) ) ;
#8561 = DIRECTION ( 'NONE',  ( -1.224646799147353207E-16, 1.000000000000000000, 0.000000000000000000 ) ) ;
#8562 = CARTESIAN_POINT ( 'NONE',  ( -3.219174618344376363E-15, 49.28125000068278894, -52.57311121191334990 ) ) ;
#8563 = DIRECTION ( 'NONE',  ( 1.000000000000000000, 0.000000000000000000, 0.000000000000000000 ) ) ;
#8564 = CARTESIAN_POINT ( 'NONE',  ( -40.45084971874737789, 25.80000000000000071, -29.38926261462365730 ) ) ;
#8565 = CARTESIAN_POINT ( 'NONE',  ( 40.34137639590981195, 21.05937500034139376, -29.30972558990011834 ) ) ;
#8566 = CARTESIAN_POINT ( 'NONE',  ( -30.90169943749474513, 41.48125000068279178, -42.53254041760200721 ) ) ;
#8567 = FACE_OUTER_BOUND ( 'NONE', #13059, .T. ) ;
#8568 = ORIENTED_EDGE ( 'NONE', *, *, #16259, .T. ) ;
#8569 = CARTESIAN_POINT ( 'NONE',  ( 30.81806926056962936, 25.15937500034139518, -42.41743335407646498 ) ) ;
#8570 = ORIENTED_EDGE ( 'NONE', *, *, #8364, .T. ) ;
#8571 = CARTESIAN_POINT ( 'NONE',  ( 50.00000000000000711, 48.90000000000000568, 16.24598481164530739 ) ) ;
#8572 = CARTESIAN_POINT ( 'NONE',  ( 15.40903463028482356, 32.45937500034138878, 47.42413220539093999 ) ) ;
#8573 = CYLINDRICAL_SURFACE ( 'NONE', #16084, 50.00000000000000000 ) ;
#8574 = FACE_OUTER_BOUND ( 'NONE', #11950, .T. ) ;
#8575 = CARTESIAN_POINT ( 'NONE',  ( 30.90169943749473802, 35.29999999999999716, -42.53254041760200721 ) ) ;
#8576 = CARTESIAN_POINT ( 'NONE',  ( -15.40903463028480580, 26.32187500034140015, 47.42413220539094709 ) ) ;
#8577 = CARTESIAN_POINT ( 'NONE',  ( 15.40903463028482356, 30.45937500034139589, 47.42413220539093999 ) ) ;
#8578 = CARTESIAN_POINT ( 'NONE',  ( 49.99999999999999289, 26.88125000068280102, -16.24598481164532160 ) ) ;
#8579 = CARTESIAN_POINT ( 'NONE',  ( 49.86468353125000164, 34.92187500034140157, -6.106662507704105588E-15 ) ) ;
#8580 = DIRECTION ( 'NONE',  ( 0.000000000000000000, 0.000000000000000000, -1.000000000000000000 ) ) ;
#8581 = AXIS2_PLACEMENT_3D ( 'NONE', #13305, #14620, #2155 ) ;
#8582 = CARTESIAN_POINT ( 'NONE',  ( -49.86468353124999453, 43.95937500034138878, 16.20201782572377525 ) ) ;
#8583 = CARTESIAN_POINT ( 'NONE',  ( -49.86468353124999453, 36.02187500034139589, 16.20201782572377525 ) ) ;
#8584 = CARTESIAN_POINT ( 'NONE',  ( -49.99999999999999289, 46.09999999999999432, 16.24598481164533226 ) ) ;
#8585 = EDGE_CURVE ( 'NONE', #286, #7551, #3344, .T. ) ;
#8587 = ORIENTED_EDGE ( 'NONE', *, *, #5123, .T. ) ;
#8586 =( BOUNDED_CURVE ( )  B_SPLINE_CURVE ( 2, ( #13230, #15639, #1669, #417, #1751, #4262, #15553, #5520, #13381, #9250, #1828, #1987, #14303 ),
 .UNSPECIFIED., .F., .F. ) 
 B_SPLINE_CURVE_WITH_KNOTS ( ( 3, 2, 2, 2, 2, 2, 3 ),
 ( 0.4833333333333333370, 0.4866666666666666918, 0.4933333333333333459, 0.5000000000000000000, 0.5066666666666667096, 0.5133333333333333082, 0.5166666666666667185 ),
 .UNSPECIFIED. ) 
 CURVE ( )  GEOMETRIC_REPRESENTATION_ITEM ( )  RATIONAL_B_SPLINE_CURVE ( ( 0.9755282581475768211, 0.9755282581475768211, 1.000000000000000000, 0.9510565162951535312, 1.000000000000000000, 0.9510565162951535312, 1.000000000000000000, 0.9510565162951535312, 1.000000000000000000, 0.9510565162951535312, 1.000000000000000000, 0.9755282581475763770, 0.9755282581475768211 ) ) 
 REPRESENTATION_ITEM ( '' )  );
#8588 = CARTESIAN_POINT ( 'NONE',  ( 30.81806926056962936, 43.15937500034139873, -42.41743335407646498 ) ) ;
#8589 = EDGE_LOOP ( 'NONE', ( #12383, #819, #10103, #2165 ) ) ;
#8590 = AXIS2_PLACEMENT_3D ( 'NONE', #8244, #4515, #6095 ) ;
#8591 = CARTESIAN_POINT ( 'NONE',  ( 40.45084971874737079, 22.98125000068279888, -29.38926261462366440 ) ) ;
#8592 = AXIS2_PLACEMENT_3D ( 'NONE', #3565, #6147, #7469 ) ;
#8593 = VERTEX_POINT ( 'NONE', #11086 ) ;
#8594 = CARTESIAN_POINT ( 'NONE',  ( -15.45084971874736368, 36.39999999999999858, 47.55282581475768211 ) ) ;
#8595 = CARTESIAN_POINT ( 'NONE',  ( 49.86468353125000164, 48.92187500034139447, -6.106662507704105588E-15 ) ) ;
#8596 = DIRECTION ( 'NONE',  ( -0.000000000000000000, 1.000000000000000000, -0.000000000000000000 ) ) ;
#8597 = CARTESIAN_POINT ( 'NONE',  ( -40.34137639590981905, 23.72187500034139873, -29.30972558990011478 ) ) ;
#8598 = CARTESIAN_POINT ( 'NONE',  ( 30.90169943749475578, 34.48125000068279888, 42.53254041760200010 ) ) ;
#8599 = CARTESIAN_POINT ( 'NONE',  ( -30.81806926056962226, 40.22187500034139873, 42.41743335407647919 ) ) ;
#8600 = CARTESIAN_POINT ( 'NONE',  ( -27.78424396843074362, 282.5058351977240250, -8.068487936864610077 ) ) ;
#8601 = ORIENTED_EDGE ( 'NONE', *, *, #10664, .F. ) ;
#8602 = CARTESIAN_POINT ( 'NONE',  ( 30.81806926056964002, 38.62187500034139731, 42.41743335407647209 ) ) ;
#8603 = LINE ( 'NONE', #2292, #11328 ) ;
#8604 = ORIENTED_EDGE ( 'NONE', *, *, #16075, .F. ) ;
#8605 = ORIENTED_EDGE ( 'NONE', *, *, #14107, .T. ) ;
#8606 = ORIENTED_EDGE ( 'NONE', *, *, #16001, .T. ) ;
#8607 = CYLINDRICAL_SURFACE ( 'NONE', #16129, 50.00000000000000000 ) ;
#8608 = CYLINDRICAL_SURFACE ( 'NONE', #3870, 50.00000000000000000 ) ;
#8610 = ADVANCED_FACE ( 'NONE', ( #3596 ), #3260, .F. ) ;
#8609 = AXIS2_PLACEMENT_3D ( 'NONE', #143, #1232, #1143 ) ;
#8611 = CARTESIAN_POINT ( 'NONE',  ( 30.90169943749475223, 26.70000000000000284, 42.53254041760199300 ) ) ;
#8612 = LINE ( 'NONE', #7465, #8994 ) ;
#8613 = CARTESIAN_POINT ( 'NONE',  ( -15.40903463028481646, 39.45937500034139589, -47.42413220539093999 ) ) ;
#8614 = CARTESIAN_POINT ( 'NONE',  ( -40.34137639590981195, 44.05937500034139731, 29.30972558990012189 ) ) ;
#8615 = CARTESIAN_POINT ( 'NONE',  ( -49.99999999999999289, 29.89999999999999858, -16.24598481164531449 ) ) ;
#8616 = DIRECTION ( 'NONE',  ( 0.000000000000000000, -5.551115123125782702E-17, 1.000000000000000000 ) ) ;
#8617 = SURFACE_STYLE_USAGE ( .BOTH. , #6392 ) ;
#8618 = DIRECTION ( 'NONE',  ( 0.000000000000000000, 0.000000000000000000, 1.000000000000000000 ) ) ;
#8619 = EDGE_CURVE ( 'NONE', #10949, #10705, #10913, .T. ) ;
#8620 = CARTESIAN_POINT ( 'NONE',  ( 6.123233995736766085E-15, 25.00000000000000000, 50.00000000000000000 ) ) ;
#8621 = LINE ( 'NONE', #13777, #8558 ) ;
#8622 = AXIS2_PLACEMENT_3D ( 'NONE', #2193, #3288, #12438 ) ;
#8623 = ORIENTED_EDGE ( 'NONE', *, *, #5916, .T. ) ;
#8624 = VECTOR ( 'NONE', #7648, 1000.000000000000000 ) ;
#8625 = CARTESIAN_POINT ( 'NONE',  ( -3.210462471511496205E-15, 27.35937500034139802, -52.43083105670540789 ) ) ;
#8626 = CARTESIAN_POINT ( 'NONE',  ( -7.919222016226804328, 48.22999571913595673, 50.00000000000000000 ) ) ;
#8627 = EDGE_CURVE ( 'NONE', #2051, #10856, #10237, .T. ) ;
#8629 = ORIENTED_EDGE ( 'NONE', *, *, #5714, .T. ) ;
#8628 = PRODUCT_RELATED_PRODUCT_CATEGORY ( 'part', '', ( #5621 ) ) ;
#8630 = ORIENTED_EDGE ( 'NONE', *, *, #15556, .F. ) ;
#8631 = CARTESIAN_POINT ( 'NONE',  ( 49.99999999999999289, 36.88125000068279036, -16.24598481164532160 ) ) ;
#8632 = CARTESIAN_POINT ( 'NONE',  ( 0.5000000000000009992, 31.99999999999998579, 101.0000000000000000 ) ) ;
#8633 = DIRECTION ( 'NONE',  ( 0.000000000000000000, -1.000000000000000000, 0.000000000000000000 ) ) ;
#8634 = EDGE_LOOP ( 'NONE', ( #2204, #4413, #11059, #2764, #1956, #3921 ) ) ;
#8635 = CARTESIAN_POINT ( 'NONE',  ( -49.99999999999999289, 47.88125000068281167, 16.24598481164533226 ) ) ;
#8636 = CARTESIAN_POINT ( 'NONE',  ( -17.11764542475608053, 21.20361710786370324, 101.3333374614808662 ) ) ;
#8637 = EDGE_CURVE ( 'NONE', #10236, #2273, #13928, .T. ) ;
#8638 = DIRECTION ( 'NONE',  ( -0.9361168066628590134, 0.08189960831908912886, -0.3420201433256691570 ) ) ;
#8639 = CARTESIAN_POINT ( 'NONE',  ( -16.48218589020113001, 28.38111794481753236, 101.0000000000000000 ) ) ;
#8640 = AXIS2_PLACEMENT_3D ( 'NONE', #1865, #3036, #14344 ) ;
#8641 = DIRECTION ( 'NONE',  ( 0.5877852522924688072, 0.8090169943749505599, 0.000000000000000000 ) ) ;
#8642 = CARTESIAN_POINT ( 'NONE',  ( 20.00000000000000000, 287.0000000000000568, -2.499999999999999556 ) ) ;
#8643 = DIRECTION ( 'NONE',  ( -0.000000000000000000, -1.000000000000000000, -0.000000000000000000 ) ) ;
#8644 =( GEOMETRIC_REPRESENTATION_CONTEXT ( 3 ) GLOBAL_UNCERTAINTY_ASSIGNED_CONTEXT ( ( #1918 ) ) GLOBAL_UNIT_ASSIGNED_CONTEXT ( ( #12798, #6492, #16463 ) ) REPRESENTATION_CONTEXT ( 'NONE', 'WORKASPACE' ) );
#8645 = CARTESIAN_POINT ( 'NONE',  ( -6.668400408272873429E-15, 49.50000000000000000, -50.00000000000000000 ) ) ;
#8646 = CARTESIAN_POINT ( 'NONE',  ( 49.99999999999999289, 48.88125000068279746, -16.24598481164532160 ) ) ;
#8647 = CARTESIAN_POINT ( 'NONE',  ( 0.000000000000000000, 22.50000000000000000, 102.0000000000000142 ) ) ;
#8648 = EDGE_CURVE ( 'NONE', #1840, #14050, #14717, .T. ) ;
#8649 = CARTESIAN_POINT ( 'NONE',  ( 15.45084971874736723, 27.40000000000000213, -47.55282581475768211 ) ) ;
#8650 = CARTESIAN_POINT ( 'NONE',  ( 30.81806926056962936, 21.15937500034140228, -42.41743335407647209 ) ) ;
#8651 = CARTESIAN_POINT ( 'NONE',  ( 5.179451399591075145, 14.52044592729181538, 101.0000000000000000 ) ) ;
#8652 = B_SPLINE_CURVE_WITH_KNOTS ( 'NONE', 3,
 ( #15301, #3923, #14053, #6259 ),
 .UNSPECIFIED., .F., .F.,
 ( 4, 4 ),
 ( 0.009967034006374431848, 0.01711986125270675146 ),
 .UNSPECIFIED. ) ;
#8653 = CARTESIAN_POINT ( 'NONE',  ( -49.86468353124999453, 45.95937500034138878, 16.20201782572377525 ) ) ;
#8654 = ORIENTED_EDGE ( 'NONE', *, *, #14649, .T. ) ;
#8655 = VECTOR ( 'NONE', #8852, 1000.000000000000000 ) ;
#8656 = VECTOR ( 'NONE', #8069, 999.9999999999998863 ) ;
#8657 = AXIS2_PLACEMENT_3D ( 'NONE', #3347, #2251, #12414 ) ;
#8658 = CARTESIAN_POINT ( 'NONE',  ( 9.574901606694759531E-15, 52.00000000000001421, -2.191293403013901163E-14 ) ) ;
#8659 = ORIENTED_EDGE ( 'NONE', *, *, #1633, .T. ) ;
#8660 = AXIS2_PLACEMENT_3D ( 'NONE', #1382, #1053, #7635 ) ;
#8661 = CARTESIAN_POINT ( 'NONE',  ( -14.90544456622763470, 13.31698729810771376, 102.0000000000000142 ) ) ;
#8662 = CARTESIAN_POINT ( 'NONE',  ( 9.631387414534489405E-15, 34.35937500034139447, 52.43083105670540789 ) ) ;
#8663 = ADVANCED_FACE ( 'NONE', ( #11480 ), #15300, .F. ) ;
#8664 = CARTESIAN_POINT ( 'NONE',  ( 9.151574469205522533, 1.945227203041487218, 101.0000000000000000 ) ) ;
#8665 = CARTESIAN_POINT ( 'NONE',  ( 0.000000000000000000, 20.00000000000000355, 0.000000000000000000 ) ) ;
#8666 = CARTESIAN_POINT ( 'NONE',  ( -6.725310538855818976, 29.22831317314782851, 102.0000000000000142 ) ) ;
#8667 = DIRECTION ( 'NONE',  ( -0.000000000000000000, -1.000000000000000000, -0.000000000000000000 ) ) ;
#8668 = CARTESIAN_POINT ( 'NONE',  ( 40.34137639590981195, 23.12187500034139731, -29.30972558990011834 ) ) ;
#8669 = CARTESIAN_POINT ( 'NONE',  ( -15.40903463028480580, 32.25937500034140015, 47.42413220539094709 ) ) ;
#8670 = VECTOR ( 'NONE', #256, 1000.000000000000000 ) ;
#8671 = VECTOR ( 'NONE', #15204, 1000.000000000000000 ) ;
#8672 = DIRECTION ( 'NONE',  ( -0.4067366430757887175, -0.9135454576426059736, 0.000000000000000000 ) ) ;
#8673 = CARTESIAN_POINT ( 'NONE',  ( 30.81806926056962936, 37.22187500034139163, -42.41743335407646498 ) ) ;
#8675 = EDGE_CURVE ( 'NONE', #15483, #2271, #13162, .T. ) ;
#8674 = VECTOR ( 'NONE', #411, 1000.000000000000000 ) ;
#8676 = DIRECTION ( 'NONE',  ( -0.000000000000000000, 1.000000000000000000, -0.000000000000000000 ) ) ;
#8677 = CARTESIAN_POINT ( 'NONE',  ( 40.34137639590981905, 40.65937500034139873, 29.30972558990010768 ) ) ;
#8678 = CARTESIAN_POINT ( 'NONE',  ( -3.210462471511496205E-15, 35.42187500034140157, -52.43083105670540789 ) ) ;
#8679 = CARTESIAN_POINT ( 'NONE',  ( 30.90169943749474157, 45.29999999999999005, -42.53254041760200721 ) ) ;
#8680 = ORIENTED_EDGE ( 'NONE', *, *, #5004, .F. ) ;
#8681 = CARTESIAN_POINT ( 'NONE',  ( -40.34137639590981905, 45.65937500034139873, -29.30972558990011478 ) ) ;
#8682 = VECTOR ( 'NONE', #15780, 1000.000000000000114 ) ;
#8683 = ORIENTED_EDGE ( 'NONE', *, *, #10581, .F. ) ;
#8684 = EDGE_CURVE ( 'NONE', #16436, #2250, #5183, .T. ) ;
#8685 = CARTESIAN_POINT ( 'NONE',  ( 9.657523855033129090E-15, 26.28125000068279604, 52.57311121191334990 ) ) ;
#8686 = CARTESIAN_POINT ( 'NONE',  ( -2.547328955960238000E-13, 24.49999999999999289, 49.99999999999999289 ) ) ;
#8687 = CARTESIAN_POINT ( 'NONE',  ( -37.77664397204053159, 40.00000000000000711, -13.15010152849376190 ) ) ;
#8688 = CARTESIAN_POINT ( 'NONE',  ( 30.81806926056962936, 45.22187500034139873, -42.41743335407647209 ) ) ;
#8689 = DIRECTION ( 'NONE',  ( -0.08715574274765824914, 0.9961946980917455452, 0.000000000000000000 ) ) ;
#8690 = CARTESIAN_POINT ( 'NONE',  ( 30.81806926056962936, 23.22187500034139163, -42.41743335407647209 ) ) ;
#8691 = CARTESIAN_POINT ( 'NONE',  ( 40.45084971874737079, 24.98125000068279888, -29.38926261462366440 ) ) ;
#8692 =( BOUNDED_CURVE ( )  B_SPLINE_CURVE ( 3, ( #8296, #14680, #5978, #3400 ),
 .UNSPECIFIED., .F., .T. ) 
 B_SPLINE_CURVE_WITH_KNOTS ( ( 4, 4 ),
 ( 3.141592653589793116, 4.712388980384689674 ),
 .UNSPECIFIED. ) 
 CURVE ( )  GEOMETRIC_REPRESENTATION_ITEM ( )  RATIONAL_B_SPLINE_CURVE ( ( 1.000000000000000000, 0.8047378541243649375, 0.8047378541243649375, 1.000000000000000000 ) ) 
 REPRESENTATION_ITEM ( '' )  );
#8693 = CARTESIAN_POINT ( 'NONE',  ( 40.34137639590981195, 33.12187500034139731, -29.30972558990011834 ) ) ;
#8694 = CARTESIAN_POINT ( 'NONE',  ( -20.31983351293596129, 285.7035871579731179, -7.659916756467383792 ) ) ;
#8695 = CARTESIAN_POINT ( 'NONE',  ( 49.86468353125001585, 34.82187500034140015, 16.20201782572375038 ) ) ;
#8696 = CARTESIAN_POINT ( 'NONE',  ( -7.919222016226752814, 41.33250428222964246, -50.00000000000000711 ) ) ;
#8697 = ORIENTED_EDGE ( 'NONE', *, *, #16177, .T. ) ;
#8698 = VERTEX_POINT ( 'NONE', #10157 ) ;
#8699 = AXIS2_PLACEMENT_3D ( 'NONE', #10051, #3731, #8877 ) ;
#8700 = ORIENTED_EDGE ( 'NONE', *, *, #1871, .T. ) ;
#8701 = CARTESIAN_POINT ( 'NONE',  ( -49.99999999999999289, 32.10000000000000142, 16.24598481164533226 ) ) ;
#8702 = CARTESIAN_POINT ( 'NONE',  ( 30.90169943749475223, 44.69999999999999574, 42.53254041760199300 ) ) ;
#8703 = CARTESIAN_POINT ( 'NONE',  ( -40.45084971874737789, 49.58125000068280031, -29.38926261462365730 ) ) ;
#8704 = CARTESIAN_POINT ( 'NONE',  ( -20.00000000000000355, 312.0000000000000568, -7.499999999999999112 ) ) ;
#8705 = EDGE_CURVE ( 'NONE', #13696, #4877, #617, .T. ) ;
#8706 = CARTESIAN_POINT ( 'NONE',  ( 15.40903463028481113, 33.25937500034140015, -47.42413220539094709 ) ) ;
#8707 = CARTESIAN_POINT ( 'NONE',  ( 30.81806926056962936, 45.15937500034139873, -42.41743335407646498 ) ) ;
#8708 = DIRECTION ( 'NONE',  ( 3.469446951953613696E-16, 0.000000000000000000, 1.000000000000000000 ) ) ;
#8709 = MANIFOLD_SOLID_BREP ( 'Boss-Extrude5', #4967 ) ;
#8710 = SURFACE_SIDE_STYLE ('',( #13853 ) ) ;
#8711 = DIRECTION ( 'NONE',  ( -0.000000000000000000, -0.000000000000000000, -1.000000000000000000 ) ) ;
#8712 = DIRECTION ( 'NONE',  ( 0.000000000000000000, 0.000000000000000000, -1.000000000000000000 ) ) ;
#8713 = ORIENTED_EDGE ( 'NONE', *, *, #4643, .F. ) ;
#8714 = CARTESIAN_POINT ( 'NONE',  ( -30.81806926056963292, 27.55937500034139376, -42.41743335407647209 ) ) ;
#8715 = CARTESIAN_POINT ( 'NONE',  ( 9.657683769731161050, 93.19872860642226442, 1.198728606422247323 ) ) ;
#8716 = ORIENTED_EDGE ( 'NONE', *, *, #6509, .T. ) ;
#8717 = ORIENTED_EDGE ( 'NONE', *, *, #10675, .T. ) ;
#8718 = CARTESIAN_POINT ( 'NONE',  ( 49.99999999999999289, 38.88125000068279036, -16.24598481164532160 ) ) ;
#8719 = DIRECTION ( 'NONE',  ( 0.000000000000000000, 0.000000000000000000, 1.000000000000000000 ) ) ;
#8720 = CARTESIAN_POINT ( 'NONE',  ( -2.500000000000000000, 247.0000000000000284, -47.99999999999999289 ) ) ;
#8721 = VERTEX_POINT ( 'NONE', #12656 ) ;
#8722 = CARTESIAN_POINT ( 'NONE',  ( 40.45084971874737079, 38.98125000068279888, -29.38926261462366440 ) ) ;
#8723 = CARTESIAN_POINT ( 'NONE',  ( -15.45084971874737256, 37.60000000000000142, -47.55282581475767500 ) ) ;
#8724 = CIRCLE ( 'NONE', #1556, 10.00000000000000000 ) ;
#8725 = CARTESIAN_POINT ( 'NONE',  ( -40.45084971874737079, 20.20000000000000284, 29.38926261462367151 ) ) ;
#8726 = DIRECTION ( 'NONE',  ( -0.000000000000000000, -0.000000000000000000, -1.000000000000000000 ) ) ;
#8727 = CARTESIAN_POINT ( 'NONE',  ( 9.253960653386475815E-15, 98.25246584726779986, -9.080892972013931086 ) ) ;
#8728 = CARTESIAN_POINT ( 'NONE',  ( 9.397478011314830142E-15, 45.00000000000000711, -45.00000000000002842 ) ) ;
#8729 = CARTESIAN_POINT ( 'NONE',  ( 7.574663982647604321, 38.28367718720770796, 102.0000000000000142 ) ) ;
#8730 = EDGE_CURVE ( 'NONE', #7924, #9110, #3590, .T. ) ;
#8731 = FACE_OUTER_BOUND ( 'NONE', #8417, .T. ) ;
#8732 = CARTESIAN_POINT ( 'NONE',  ( 15.45084971874736723, 49.18125000068279462, -47.55282581475768211 ) ) ;
#8733 = CARTESIAN_POINT ( 'NONE',  ( 49.99999999999999289, 44.88125000068279036, -16.24598481164532160 ) ) ;
#8734 = CARTESIAN_POINT ( 'NONE',  ( 50.00000000000000711, 22.90000000000000213, 16.24598481164530739 ) ) ;
#8735 = CARTESIAN_POINT ( 'NONE',  ( 0.000000000000000000, 54.99999999999999289, -42.00000000000000711 ) ) ;
#8736 = CARTESIAN_POINT ( 'NONE',  ( -14.32166083077703966, 13.65403499491864459, 101.6666710451724214 ) ) ;
#8737 = CARTESIAN_POINT ( 'NONE',  ( 30.81806926056962936, 43.15937500034140584, -42.41743335407647209 ) ) ;
#8738 = CIRCLE ( 'NONE', #14313, 6.000000000000001776 ) ;
#8739 = ORIENTED_EDGE ( 'NONE', *, *, #14807, .F. ) ;
#8740 = CARTESIAN_POINT ( 'NONE',  ( 0.000000000000000000, 54.99999999999999289, 0.000000000000000000 ) ) ;
#8741 = VERTEX_POINT ( 'NONE', #5103 ) ;
#8742 = DIRECTION ( 'NONE',  ( 0.000000000000000000, 0.000000000000000000, -1.000000000000000000 ) ) ;
#8743 = CARTESIAN_POINT ( 'NONE',  ( -40.34137639590981195, 28.05937500034139731, 29.30972558990012189 ) ) ;
#8744 = EDGE_CURVE ( 'NONE', #404, #7399, #10220, .T. ) ;
#8745 = CARTESIAN_POINT ( 'NONE',  ( -15.45084971874736368, 20.18125000068279817, 47.55282581475768211 ) ) ;
#8746 = PLANE ( 'NONE',  #15549 ) ;
#8747 = CARTESIAN_POINT ( 'NONE',  ( 45.80914010100575240, 25.00000000000000000, -19.69865795820044951 ) ) ;
#8748 = CARTESIAN_POINT ( 'NONE',  ( 0.000000000000000000, 272.0000000000000000, 0.000000000000000000 ) ) ;
#8749 = ADVANCED_FACE ( 'NONE', ( #2995 ), #11971, .F. ) ;
#8750 = CIRCLE ( 'NONE', #4800, 5.000000000000000000 ) ;
#8751 = CARTESIAN_POINT ( 'NONE',  ( -40.34137639590981905, 23.72187500034139873, -29.30972558990011478 ) ) ;
#8752 = CARTESIAN_POINT ( 'NONE',  ( 9.631387414534489405E-15, 26.35937500034139802, 52.43083105670540789 ) ) ;
#8753 = LINE ( 'NONE', #1422, #9485 ) ;
#8754 = CARTESIAN_POINT ( 'NONE',  ( -40.34137639590981195, 34.12187500034139731, 29.30972558990012189 ) ) ;
#8755 = EDGE_CURVE ( 'NONE', #14669, #4716, #3042, .T. ) ;
#8756 = LINE ( 'NONE', #10096, #8152 ) ;
#8757 = CARTESIAN_POINT ( 'NONE',  ( -30.90169943749474868, 35.69999999999999574, -42.53254041760200721 ) ) ;
#8758 = CARTESIAN_POINT ( 'NONE',  ( 15.40903463028482356, 40.45937500034139589, 47.42413220539093999 ) ) ;
#8759 = CARTESIAN_POINT ( 'NONE',  ( -49.86468353125000164, 29.92187500034139802, 0.000000000000000000 ) ) ;
#8760 = ADVANCED_FACE ( 'NONE', ( #9324, #5592 ), #13223, .F. ) ;
#8761 = CARTESIAN_POINT ( 'NONE',  ( -40.45084971874737079, 44.20000000000000284, 29.38926261462367151 ) ) ;
#8762 = EDGE_LOOP ( 'NONE', ( #188, #10934, #15058, #11504 ) ) ;
#8763 = CARTESIAN_POINT ( 'NONE',  ( 30.81806926056962936, 37.15937500034139163, -42.41743335407646498 ) ) ;
#8764 = ORIENTED_EDGE ( 'NONE', *, *, #5533, .T. ) ;
#8765 = ORIENTED_EDGE ( 'NONE', *, *, #4809, .F. ) ;
#8766 = CARTESIAN_POINT ( 'NONE',  ( -49.99999999999999289, 23.88125000068279746, 16.24598481164533226 ) ) ;
#8767 = LINE ( 'NONE', #5211, #11279 ) ;
#8768 = CARTESIAN_POINT ( 'NONE',  ( 30.81806926056964002, 24.62187500034139731, 42.41743335407647209 ) ) ;
#8769 = LINE ( 'NONE', #6452, #3076 ) ;
#8770 = CARTESIAN_POINT ( 'NONE',  ( 9.631387414534489405E-15, 40.42187500034138736, 52.43083105670540789 ) ) ;
#8771 = CARTESIAN_POINT ( 'NONE',  ( -13.33429048796512717, 33.83343271840278277, 101.0000000000000000 ) ) ;
#8772 = CARTESIAN_POINT ( 'NONE',  ( 30.90169943749474157, 47.29999999999999716, -42.53254041760200721 ) ) ;
#8773 = CARTESIAN_POINT ( 'NONE',  ( -49.99999999999999289, 27.88125000068279746, 16.24598481164533226 ) ) ;
#8774 = CARTESIAN_POINT ( 'NONE',  ( 12.59082374547730332, 33.16401225666611197, 102.0000000000000142 ) ) ;
#8775 = EDGE_CURVE ( 'NONE', #15423, #11431, #7041, .T. ) ;
#8776 = CARTESIAN_POINT ( 'NONE',  ( 49.86468353124999453, 37.02187500034138878, -16.20201782572376459 ) ) ;
#8777 = CARTESIAN_POINT ( 'NONE',  ( -29.34550962211183744, 282.0322304394514390, -11.19101924422352035 ) ) ;
#8778 = EDGE_CURVE ( 'NONE', #11268, #11668, #6379, .T. ) ;
#8779 = CARTESIAN_POINT ( 'NONE',  ( -15.40903463028480580, 34.32187500034139305, 47.42413220539094709 ) ) ;
#8780 = DIRECTION ( 'NONE',  ( 1.224646799147353207E-16, -1.000000000000000000, 0.000000000000000000 ) ) ;
#8781 = ORIENTED_EDGE ( 'NONE', *, *, #5987, .T. ) ;
#8782 = ORIENTED_EDGE ( 'NONE', *, *, #5722, .T. ) ;
#8783 = FACE_OUTER_BOUND ( 'NONE', #1983, .T. ) ;
#8784 = DIRECTION ( 'NONE',  ( -0.000000000000000000, -1.000000000000000000, -0.000000000000000000 ) ) ;
#8785 = DIRECTION ( 'NONE',  ( -0.5877852522924797984, 0.8090169943749424553, 0.000000000000000000 ) ) ;
#8786 = DIRECTION ( 'NONE',  ( -0.000000000000000000, -0.000000000000000000, 1.000000000000000000 ) ) ;
#8787 = CARTESIAN_POINT ( 'NONE',  ( 30.81806926056964002, 30.55937500034139731, 42.41743335407647209 ) ) ;
#8788 =( BOUNDED_CURVE ( )  B_SPLINE_CURVE ( 2, ( #4668, #9741, #2233, #16211, #4843, #15960, #4763, #9820, #3579, #14617, #1902, #6996, #3417 ),
 .UNSPECIFIED., .F., .T. ) 
 B_SPLINE_CURVE_WITH_KNOTS ( ( 3, 2, 2, 2, 2, 2, 3 ),
 ( 0.7166666666666666741, 0.7199999999999999734, 0.7266666666666666829, 0.7333333333333332815, 0.7399999999999999911, 0.7466666666666667007, 0.7500000000000000000 ),
 .UNSPECIFIED. ) 
 CURVE ( )  GEOMETRIC_REPRESENTATION_ITEM ( )  RATIONAL_B_SPLINE_CURVE ( ( 0.9755282581475768211, 0.9755282581475768211, 1.000000000000000000, 0.9510565162951535312, 1.000000000000000000, 0.9510565162951535312, 1.000000000000000000, 0.9510565162951535312, 1.000000000000000000, 0.9510565162951535312, 1.000000000000000000, 0.9755282581475768211, 0.9755282581475768211 ) ) 
 REPRESENTATION_ITEM ( '' )  );
#8789 = CARTESIAN_POINT ( 'NONE',  ( -40.34137639590981905, 45.72187500034139873, -29.30972558990011478 ) ) ;
#8790 = CARTESIAN_POINT ( 'NONE',  ( 7.919222016226809657, 35.22999571913594963, -50.00000000000000000 ) ) ;
#8791 = LINE ( 'NONE', #13855, #2329 ) ;
#8792 = LINE ( 'NONE', #3898, #13078 ) ;
#8793 = ORIENTED_EDGE ( 'NONE', *, *, #1717, .F. ) ;
#8794 = ADVANCED_FACE ( 'NONE', ( #6597 ), #5842, .T. ) ;
#8795 = CARTESIAN_POINT ( 'NONE',  ( -30.81806926056963292, 23.55937500034139376, -42.41743335407647209 ) ) ;
#8796 = EDGE_CURVE ( 'NONE', #9638, #13296, #9492, .T. ) ;
#8797 = ORIENTED_EDGE ( 'NONE', *, *, #16383, .F. ) ;
#8798 = DIRECTION ( 'NONE',  ( 0.000000000000000000, -1.000000000000000000, 0.000000000000000000 ) ) ;
#8799 = VERTEX_POINT ( 'NONE', #9247 ) ;
#8800 = ORIENTED_EDGE ( 'NONE', *, *, #13511, .T. ) ;
#8801 = CARTESIAN_POINT ( 'NONE',  ( 17.45639740057861644, 21.16801284050037424, 101.0000000000000000 ) ) ;
#8802 = CARTESIAN_POINT ( 'NONE',  ( 0.000000000000000000, 0.000000000000000000, 101.0000000000000000 ) ) ;
#8803 = CARTESIAN_POINT ( 'NONE',  ( 15.45084971874737789, 38.38125000068279746, 47.55282581475767500 ) ) ;
#8804 = FACE_OUTER_BOUND ( 'NONE', #7176, .T. ) ;
#8805 = SPHERICAL_SURFACE ( 'NONE', #3097, 5.000000000000000000 ) ;
#8806 = CARTESIAN_POINT ( 'NONE',  ( 0.000000000000000000, 20.00000000000000355, 0.000000000000000000 ) ) ;
#8807 = LINE ( 'NONE', #1071, #14681 ) ;
#8808 = CARTESIAN_POINT ( 'NONE',  ( 37.77664397204034685, 25.00000000000000355, -13.15010152849429481 ) ) ;
#8809 = CARTESIAN_POINT ( 'NONE',  ( -0.5000000000000000000, 245.0000000000000284, -49.99999999999999289 ) ) ;
#8810 = CARTESIAN_POINT ( 'NONE',  ( 0.000000000000000000, 261.9999999999999432, 0.000000000000000000 ) ) ;
#8811 = CARTESIAN_POINT ( 'NONE',  ( -3.219174618344376363E-15, 47.28125000068278894, -52.57311121191334990 ) ) ;
#8812 = CARTESIAN_POINT ( 'NONE',  ( 30.90169943749473802, 45.08125000068280031, -42.53254041760200721 ) ) ;
#8813 = CARTESIAN_POINT ( 'NONE',  ( -40.45084971874737079, 24.20000000000000284, 29.38926261462367151 ) ) ;
#8814 = CARTESIAN_POINT ( 'NONE',  ( -15.40903463028481646, 21.45937500034139589, -47.42413220539093999 ) ) ;
#8815 = CARTESIAN_POINT ( 'NONE',  ( -7.919222016226838967, 44.44874571845315359, 49.99999999999999289 ) ) ;
#8816 = CARTESIAN_POINT ( 'NONE',  ( -40.34137639590981905, 41.65937500034139873, -29.30972558990011478 ) ) ;
#8817 = VERTEX_POINT ( 'NONE', #3414 ) ;
#8818 = CARTESIAN_POINT ( 'NONE',  ( 40.45084971874737789, 42.58125000068280031, 29.38926261462365375 ) ) ;
#8819 = ORIENTED_EDGE ( 'NONE', *, *, #8165, .F. ) ;
#8820 = CARTESIAN_POINT ( 'NONE',  ( -43.87482193696061472, 267.0000000000000000, 10.00000000000000178 ) ) ;
#8821 = CARTESIAN_POINT ( 'NONE',  ( -3.210462471511496205E-15, 27.35937500034139802, -52.43083105670540789 ) ) ;
#8822 = VECTOR ( 'NONE', #13131, 1000.000000000000000 ) ;
#8823 = CARTESIAN_POINT ( 'NONE',  ( 2.600676159226420495E-13, 33.49999999999999289, -49.99999999999999289 ) ) ;
#8824 = CARTESIAN_POINT ( 'NONE',  ( -10.22384026579626060, 36.71443566863956676, 92.96696093445143561 ) ) ;
#8825 = CARTESIAN_POINT ( 'NONE',  ( 48.11476475577527623, 25.00000000000000000, -13.09518440664933436 ) ) ;
#8826 = CARTESIAN_POINT ( 'NONE',  ( 15.40903463028482356, 32.52187500034139589, 47.42413220539093999 ) ) ;
#8827 = CARTESIAN_POINT ( 'NONE',  ( -2.464234863135557063, 13.31155363843772932, 101.0000000000000000 ) ) ;
#8828 = CARTESIAN_POINT ( 'NONE',  ( -40.34137639590981195, 24.12187500034139731, 29.30972558990012189 ) ) ;
#8829 = CARTESIAN_POINT ( 'NONE',  ( 15.40903463028482356, 20.45937500034139589, 47.42413220539093999 ) ) ;
#8830 = DIRECTION ( 'NONE',  ( -0.000000000000000000, -1.000000000000000000, -0.000000000000000000 ) ) ;
#8831 = CARTESIAN_POINT ( 'NONE',  ( 15.40903463028482356, 32.52187500034139589, 47.42413220539093999 ) ) ;
#8832 = DIRECTION ( 'NONE',  ( -0.000000000000000000, 0.000000000000000000, 1.000000000000000000 ) ) ;
#8833 = CARTESIAN_POINT ( 'NONE',  ( -40.45084971874737789, 33.80000000000000426, -29.38926261462365730 ) ) ;
#8834 = CARTESIAN_POINT ( 'NONE',  ( 15.40903463028481113, 39.25937500034140015, -47.42413220539094709 ) ) ;
#8835 = CARTESIAN_POINT ( 'NONE',  ( -40.34137639590981195, 32.12187500034140442, 29.30972558990012189 ) ) ;
#8836 =( BOUNDED_CURVE ( )  B_SPLINE_CURVE ( 2, ( #5263, #10393, #7892, #1489, #14284, #6829, #6583, #10641, #3059, #7974, #9063, #15693, #8139 ),
 .UNSPECIFIED., .F., .T. ) 
 B_SPLINE_CURVE_WITH_KNOTS ( ( 3, 2, 2, 2, 2, 2, 3 ),
 ( 0.01666666666666666644, 0.02000000000000000042, 0.02666666666666666838, 0.03333333333333333287, 0.04000000000000000083, 0.04666666666666666879, 0.05000000000000000278 ),
 .UNSPECIFIED. ) 
 CURVE ( )  GEOMETRIC_REPRESENTATION_ITEM ( )  RATIONAL_B_SPLINE_CURVE ( ( 0.9755282581475768211, 0.9755282581475768211, 1.000000000000000000, 0.9510565162951535312, 1.000000000000000000, 0.9510565162951535312, 1.000000000000000000, 0.9510565162951535312, 1.000000000000000000, 0.9510565162951535312, 1.000000000000000000, 0.9755282581475768211, 0.9755282581475768211 ) ) 
 REPRESENTATION_ITEM ( '' )  );
#8837 = EDGE_CURVE ( 'NONE', #4024, #1001, #8478, .T. ) ;
#8838 = AXIS2_PLACEMENT_3D ( 'NONE', #11946, #14352, #544 ) ;
#8839 = ADVANCED_FACE ( 'NONE', ( #9643 ), #4579, .F. ) ;
#8840 = CARTESIAN_POINT ( 'NONE',  ( -15.45084971874736368, 48.40000000000000568, 47.55282581475768211 ) ) ;
#8841 = ORIENTED_EDGE ( 'NONE', *, *, #11380, .F. ) ;
#8842 = CARTESIAN_POINT ( 'NONE',  ( -49.86468353124999453, 37.75937500034140015, -16.20201782572375393 ) ) ;
#8843 = ORIENTED_EDGE ( 'NONE', *, *, #13016, .T. ) ;
#8844 = ORIENTED_EDGE ( 'NONE', *, *, #787, .F. ) ;
#8845 = LINE ( 'NONE', #1439, #13184 ) ;
#8847 = ADVANCED_FACE ( 'NONE', ( #13544, #9737 ), #12140, .F. ) ;
#8846 = CARTESIAN_POINT ( 'NONE',  ( -40.34137639590981905, 49.65937500034139873, -29.30972558990011478 ) ) ;
#8848 = MANIFOLD_SOLID_BREP ( 'Boss-Extrude2', #12910 ) ;
#8849 = FACE_OUTER_BOUND ( 'NONE', #6573, .T. ) ;
#8850 = CARTESIAN_POINT ( 'NONE',  ( 15.40903463028481113, 25.32187500034139660, -47.42413220539094709 ) ) ;
#8851 = AXIS2_PLACEMENT_3D ( 'NONE', #9576, #3170, #15964 ) ;
#8852 = DIRECTION ( 'NONE',  ( -0.000000000000000000, -0.7890408728378112135, 0.6143407043256575717 ) ) ;
#8853 = EDGE_CURVE ( 'NONE', #605, #9440, #7077, .T. ) ;
#8854 = CARTESIAN_POINT ( 'NONE',  ( -40.34137639590981905, 43.72187500034139873, -29.30972558990011478 ) ) ;
#8855 = CARTESIAN_POINT ( 'NONE',  ( -49.99999999999999289, 25.88125000068279746, 16.24598481164533226 ) ) ;
#8856 = CARTESIAN_POINT ( 'NONE',  ( 30.90169943749475578, 48.69999999999999574, 42.53254041760200010 ) ) ;
#8857 = CARTESIAN_POINT ( 'NONE',  ( 50.00000000000000000, 30.78125000068279959, -6.123233995736766085E-15 ) ) ;
#8858 = CARTESIAN_POINT ( 'NONE',  ( -49.86468353124999453, 47.82187500034140015, -16.20201782572375393 ) ) ;
#8859 = ADVANCED_FACE ( 'NONE', ( #11152 ), #15521, .F. ) ;
#8860 = CARTESIAN_POINT ( 'NONE',  ( 30.81806926056962936, 35.22187500034138452, -42.41743335407647209 ) ) ;
#8861 = CARTESIAN_POINT ( 'NONE',  ( -7.500000000000000000, 25.00000000000000355, -39.29058411375427795 ) ) ;
#8862 = VECTOR ( 'NONE', #9744, 1000.000000000000000 ) ;
#8863 = B_SPLINE_CURVE_WITH_KNOTS ( 'NONE', 3,
 ( #4089, #16401, #5110, #8910, #12661, #13974, #15137, #10330, #12900, #9159, #3928, #8824, #14216, #2841, #7909, #1590, #253, #2502, #1510, #1257, #4010, #7747, #15388, #6602, #12986, #83, #1337, #3764 ),
 .UNSPECIFIED., .F., .F.,
 ( 4, 2, 2, 2, 2, 2, 2, 2, 2, 2, 2, 2, 2, 4 ),
 ( 0.06961014663733354479, 0.07132520376916648419, 0.07304026090099940971, 0.07475531803283234911, 0.07647037516466527463, 0.07990048942833113954, 0.08161554656016407894, 0.08333060369199700446, 0.08676071795566286937, 0.08847577508749582265, 0.09019083221932876204, 0.09362094648299464084, 0.09533600361482758023, 0.09705106074666051963 ),
 .UNSPECIFIED. ) ;
#8864 = CARTESIAN_POINT ( 'NONE',  ( 1.036604930454412972E-14, 98.25246584726775723, 9.080892972013893782 ) ) ;
#8865 = ORIENTED_EDGE ( 'NONE', *, *, #8420, .F. ) ;
#8866 = EDGE_LOOP ( 'NONE', ( #9951, #3324, #9619, #2142 ) ) ;
#8867 = CARTESIAN_POINT ( 'NONE',  ( -5.823736356558307894E-14, 44.50000000000000000, 50.00000000000000000 ) ) ;
#8868 = DIRECTION ( 'NONE',  ( 0.000000000000000000, -1.000000000000000000, 0.000000000000000000 ) ) ;
#8869 = CARTESIAN_POINT ( 'NONE',  ( -7.919222016226688865, 23.33250428222964246, -50.00000000000003553 ) ) ;
#8870 = CARTESIAN_POINT ( 'NONE',  ( 49.86468353125001585, 30.75937500034139305, 16.20201782572375038 ) ) ;
#8871 = AXIS2_PLACEMENT_3D ( 'NONE', #7170, #8561, #10984 ) ;
#8872 = FILL_AREA_STYLE ('',( #12458 ) ) ;
#8873 = AXIS2_PLACEMENT_3D ( 'NONE', #1815, #4324, #6907 ) ;
#8874 = CARTESIAN_POINT ( 'NONE',  ( -30.81806926056962226, 44.22187500034139163, 42.41743335407647209 ) ) ;
#8875 = CARTESIAN_POINT ( 'NONE',  ( -7.919222016226870942, 40.44874571845315359, 49.99999999999997158 ) ) ;
#8876 = EDGE_CURVE ( 'NONE', #11431, #15423, #115, .T. ) ;
#8877 = DIRECTION ( 'NONE',  ( 0.000000000000000000, -0.000000000000000000, 1.000000000000000000 ) ) ;
#8878 = CARTESIAN_POINT ( 'NONE',  ( -7.919222016226773242, 42.44874571845315359, 50.00000000000000711 ) ) ;
#8879 = ORIENTED_EDGE ( 'NONE', *, *, #29, .T. ) ;
#8880 = CARTESIAN_POINT ( 'NONE',  ( 49.86468353125001585, 22.75937500034139660, 16.20201782572375038 ) ) ;
#8881 = VERTEX_POINT ( 'NONE', #13705 ) ;
#8882 = DIRECTION ( 'NONE',  ( -0.3535533905932803922, 0.7071067811865487940, -0.6123724356957891413 ) ) ;
#8883 = VERTEX_POINT ( 'NONE', #2149 ) ;
#8884 = ORIENTED_EDGE ( 'NONE', *, *, #6334, .F. ) ;
#8885 = AXIS2_PLACEMENT_3D ( 'NONE', #7406, #3666, #14785 ) ;
#8886 = LINE ( 'NONE', #13944, #4144 ) ;
#8887 = LINE ( 'NONE', #2569, #8624 ) ;
#8888 =( NAMED_UNIT ( * ) PLANE_ANGLE_UNIT ( ) SI_UNIT ( $, .RADIAN. ) );
#8889 = CYLINDRICAL_SURFACE ( 'NONE', #7957, 50.00000000000000000 ) ;
#8890 = CARTESIAN_POINT ( 'NONE',  ( 8.446640517145639571E-15, 26.50000000000000000, 50.00000000000000000 ) ) ;
#8891 = LINE ( 'NONE', #13950, #4971 ) ;
#8892 = PLANE ( 'NONE',  #9389 ) ;
#8893 = CARTESIAN_POINT ( 'NONE',  ( 30.90169943749473802, 25.08125000068279675, -42.53254041760200721 ) ) ;
#8894 = EDGE_CURVE ( 'NONE', #384, #10597, #10929, .T. ) ;
#8895 = DIRECTION ( 'NONE',  ( 0.000000000000000000, 0.000000000000000000, -1.000000000000000000 ) ) ;
#8896 = CARTESIAN_POINT ( 'NONE',  ( -3.219174618344376363E-15, 39.28125000068279604, -52.57311121191334990 ) ) ;
#8897 = CARTESIAN_POINT ( 'NONE',  ( -5.823736356558307894E-14, 44.28125000068280315, 50.00000000000000000 ) ) ;
#8898 = AXIS2_PLACEMENT_3D ( 'NONE', #8740, #10323, #16465 ) ;
#8899 = CARTESIAN_POINT ( 'NONE',  ( -15.45084971874736368, 20.40000000000000213, 47.55282581475768211 ) ) ;
#8900 = CARTESIAN_POINT ( 'NONE',  ( -40.45084971874737789, 25.80000000000000071, -29.38926261462365730 ) ) ;
#8901 = ORIENTED_EDGE ( 'NONE', *, *, #5743, .F. ) ;
#8902 = CARTESIAN_POINT ( 'NONE',  ( 49.86468353125000164, 40.85937500034139447, -6.106662507704105588E-15 ) ) ;
#8903 = EDGE_LOOP ( 'NONE', ( #8551, #6042, #10575, #14612 ) ) ;
#8904 = CARTESIAN_POINT ( 'NONE',  ( 0.000000000000000000, 22.50000000000000000, 101.0000000000000000 ) ) ;
#8905 = DIRECTION ( 'NONE',  ( 0.000000000000000000, 1.000000000000000000, 0.000000000000000000 ) ) ;
#8906 = CARTESIAN_POINT ( 'NONE',  ( -15.40903463028480580, 26.25937500034140015, 47.42413220539094709 ) ) ;
#8907 = AXIS2_PLACEMENT_3D ( 'NONE', #3054, #2814, #10637 ) ;
#8908 = ORIENTED_EDGE ( 'NONE', *, *, #1924, .T. ) ;
#8909 = CARTESIAN_POINT ( 'NONE',  ( 7.919222016226822092, 26.55125428154684641, 49.99999999999999289 ) ) ;
#8910 = CARTESIAN_POINT ( 'NONE',  ( -2.303005534166477464, 39.85734974871404290, 92.94531063127084280 ) ) ;
#8911 = CARTESIAN_POINT ( 'NONE',  ( 46.00435827497725683, 24.99999999999998579, -19.23833313609256734 ) ) ;
#8912 = CARTESIAN_POINT ( 'NONE',  ( -49.86468353124999453, 32.02187500034139589, 16.20201782572377169 ) ) ;
#8913 = CARTESIAN_POINT ( 'NONE',  ( 40.45084971874737789, 30.58125000068279675, 29.38926261462365375 ) ) ;
#8914 = CARTESIAN_POINT ( 'NONE',  ( 15.40903463028481113, 23.25937500034139660, -47.42413220539094709 ) ) ;
#8915 = CARTESIAN_POINT ( 'NONE',  ( 7.919222016226854954, 42.55125428154684641, 49.99999999999998579 ) ) ;
#8916 = CARTESIAN_POINT ( 'NONE',  ( 9.631387414534489405E-15, 34.42187500034139447, 52.43083105670540789 ) ) ;
#8917 = CARTESIAN_POINT ( 'NONE',  ( -7.919222016226934890, 30.22999571913595318, 49.99999999999996447 ) ) ;
#8918 = CARTESIAN_POINT ( 'NONE',  ( 9.657523855033129090E-15, 32.50000000000000000, 52.57311121191334990 ) ) ;
#8919 = CARTESIAN_POINT ( 'NONE',  ( -3.210462471511496205E-15, 41.35937500034138736, -52.43083105670540789 ) ) ;
#8920 = AXIS2_PLACEMENT_3D ( 'NONE', #6884, #5631, #291 ) ;
#8921 = CARTESIAN_POINT ( 'NONE',  ( 49.86468353125000164, 32.92187500034139447, -6.106662507704105588E-15 ) ) ;
#8922 = VECTOR ( 'NONE', #6601, 1000.000000000000000 ) ;
#8923 = AXIS2_PLACEMENT_3D ( 'NONE', #15504, #14173, #1008 ) ;
#8924 = CARTESIAN_POINT ( 'NONE',  ( 40.45084971874737079, 47.20000000000000284, -29.38926261462366440 ) ) ;
#8925 = ORIENTED_EDGE ( 'NONE', *, *, #9653, .F. ) ;
#8926 = ORIENTED_EDGE ( 'NONE', *, *, #4317, .F. ) ;
#8927 = EDGE_CURVE ( 'NONE', #11268, #13562, #13621, .T. ) ;
#8928 = PRODUCT_DEFINITION_CONTEXT ( 'detailed design', #2077, 'design' ) ;
#8929 = CARTESIAN_POINT ( 'NONE',  ( -40.34137639590981195, 36.05937500034139731, 29.30972558990012189 ) ) ;
#8930 = EDGE_CURVE ( 'NONE', #15550, #8086, #8358, .T. ) ;
#8931 = ORIENTED_EDGE ( 'NONE', *, *, #7914, .T. ) ;
#8932 = EDGE_LOOP ( 'NONE', ( #1805, #13923, #8683, #4943 ) ) ;
#8933 = CARTESIAN_POINT ( 'NONE',  ( 24.99999979514750947, 287.0011897833099397, -7.499999667114691349 ) ) ;
#8934 = CARTESIAN_POINT ( 'NONE',  ( -15.40903463028481646, 47.45937500034139589, -47.42413220539093999 ) ) ;
#8935 = AXIS2_PLACEMENT_3D ( 'NONE', #3528, #3273, #10925 ) ;
#8936 = FACE_OUTER_BOUND ( 'NONE', #7554, .T. ) ;
#8937 = CONICAL_SURFACE ( 'NONE', #14492, 16.50000000000000711, 0.7853981633974447263 ) ;
#8938 = VECTOR ( 'NONE', #729, 1000.000000000000000 ) ;
#8939 = CARTESIAN_POINT ( 'NONE',  ( 40.34137639590981195, 21.12187500034139376, -29.30972558990011834 ) ) ;
#8940 = VECTOR ( 'NONE', #10313, 1000.000000000000114 ) ;
#8941 = DIRECTION ( 'NONE',  ( -0.000000000000000000, 1.000000000000000000, -0.000000000000000000 ) ) ;
#8942 = CARTESIAN_POINT ( 'NONE',  ( -40.34137639590981905, 41.72187500034139873, -29.30972558990011478 ) ) ;
#8943 = DIRECTION ( 'NONE',  ( -0.000000000000000000, -1.000000000000000000, -0.000000000000000000 ) ) ;
#8944 = CARTESIAN_POINT ( 'NONE',  ( -3.219174618344376363E-15, 49.50000000000000711, -52.57311121191334990 ) ) ;
#8945 = CARTESIAN_POINT ( 'NONE',  ( 30.90169943749475578, 28.48125000068280244, 42.53254041760200010 ) ) ;
#8946 = EDGE_CURVE ( 'NONE', #1083, #9777, #5356, .T. ) ;
#8947 = PRODUCT_RELATED_PRODUCT_CATEGORY ( 'part', '', ( #1877 ) ) ;
#8948 = CARTESIAN_POINT ( 'NONE',  ( 30.81806926056964002, 48.62187500034139731, 42.41743335407647209 ) ) ;
#8949 = CARTESIAN_POINT ( 'NONE',  ( 40.34137639590981905, 32.72187500034139873, 29.30972558990010768 ) ) ;
#8950 = CIRCLE ( 'NONE', #7093, 42.00000000000000711 ) ;
#8951 = CARTESIAN_POINT ( 'NONE',  ( 1.034642314881058238E-14, 101.0808929720139417, 9.080892972013893782 ) ) ;
#8952 = EDGE_LOOP ( 'NONE', ( #3100, #6157, #2047, #15835 ) ) ;
#8953 = ORIENTED_EDGE ( 'NONE', *, *, #9362, .F. ) ;
#8954 = DIRECTION ( 'NONE',  ( 0.1045284632676436315, 0.9945218953682742891, 0.000000000000000000 ) ) ;
#8955 = PLANE ( 'NONE',  #935 ) ;
#8956 = EDGE_CURVE ( 'NONE', #13519, #7238, #9977, .T. ) ;
#8957 = LINE ( 'NONE', #2548, #9983 ) ;
#8958 = CARTESIAN_POINT ( 'NONE',  ( 37.77664397204061686, 25.00000000000000355, 13.15010152849349900 ) ) ;
#8959 = AXIS2_PLACEMENT_3D ( 'NONE', #996, #8323, #13388 ) ;
#8960 = CARTESIAN_POINT ( 'NONE',  ( 9.631387414534489405E-15, 32.35937500034139447, 52.43083105670540789 ) ) ;
#8961 = AXIS2_PLACEMENT_3D ( 'NONE', #12712, #2568, #13864 ) ;
#8962 = CARTESIAN_POINT ( 'NONE',  ( -49.86468353124999453, 45.82187500034140015, -16.20201782572375393 ) ) ;
#8963 = PRESENTATION_STYLE_ASSIGNMENT (( #8617 ) ) ;
#8964 = CARTESIAN_POINT ( 'NONE',  ( 2.500000000000000000, 247.0000000000000284, 47.99999999999999289 ) ) ;
#8965 = CARTESIAN_POINT ( 'NONE',  ( -40.45084971874737079, 35.98125000068279888, 29.38926261462367151 ) ) ;
#8966 = CARTESIAN_POINT ( 'NONE',  ( 4.883629682448357379, 95.00500682027384869, 5.000000000000000888 ) ) ;
#8967 = VERTEX_POINT ( 'NONE', #2480 ) ;
#8968 = ADVANCED_FACE ( 'NONE', ( #2726 ), #15115, .F. ) ;
#8969 = CARTESIAN_POINT ( 'NONE',  ( 15.40903463028482356, 48.52187500034140299, 47.42413220539093999 ) ) ;
#8970 = VECTOR ( 'NONE', #889, 1000.000000000000000 ) ;
#8971 = ORIENTED_EDGE ( 'NONE', *, *, #3489, .F. ) ;
#8972 = CARTESIAN_POINT ( 'NONE',  ( -15.45084971874737256, 45.38125000068279746, -47.55282581475767500 ) ) ;
#8973 = ORIENTED_EDGE ( 'NONE', *, *, #3067, .F. ) ;
#8974 = ORIENTED_EDGE ( 'NONE', *, *, #8457, .F. ) ;
#8975 = DIRECTION ( 'NONE',  ( -0.000000000000000000, -1.000000000000000000, -0.000000000000000000 ) ) ;
#8976 = LINE ( 'NONE', #12964, #9831 ) ;
#8977 = CARTESIAN_POINT ( 'NONE',  ( 0.000000000000000000, 22.50000000000000000, 102.0000000000000142 ) ) ;
#8978 = FACE_OUTER_BOUND ( 'NONE', #16243, .T. ) ;
#8979 = CARTESIAN_POINT ( 'NONE',  ( 30.00000000000000000, 282.0000000000000000, 12.50000000000000178 ) ) ;
#8980 = CARTESIAN_POINT ( 'NONE',  ( -1.240322475938754499E-13, 38.50000000000000711, 50.00000000000000000 ) ) ;
#8981 = FACE_OUTER_BOUND ( 'NONE', #455, .T. ) ;
#8982 =( REPRESENTATION_RELATIONSHIP ('NONE','NONE', #6178, #329 ) REPRESENTATION_RELATIONSHIP_WITH_TRANSFORMATION ( #1869 )SHAPE_REPRESENTATION_RELATIONSHIP( ) );
#8983 = DIRECTION ( 'NONE',  ( -0.000000000000000000, 1.000000000000000000, -0.000000000000000000 ) ) ;
#8984 = CARTESIAN_POINT ( 'NONE',  ( 30.90169943749474157, 39.08125000068280031, -42.53254041760200721 ) ) ;
#8985 = CARTESIAN_POINT ( 'NONE',  ( 0.000000000000000000, 22.50000000000000000, 101.0000000000000000 ) ) ;
#8986 = CARTESIAN_POINT ( 'NONE',  ( 15.45084971874737789, 22.60000000000000142, 47.55282581475767500 ) ) ;
#8987 =( NAMED_UNIT ( * ) PLANE_ANGLE_UNIT ( ) SI_UNIT ( $, .RADIAN. ) );
#8988 = EDGE_CURVE ( 'NONE', #11555, #13617, #13865, .T. ) ;
#8989 = EDGE_LOOP ( 'NONE', ( #14132, #8351, #1953 ) ) ;
#8990 = ADVANCED_FACE ( 'NONE', ( #10223 ), #6484, .F. ) ;
#8991 = CARTESIAN_POINT ( 'NONE',  ( -15.40903463028480580, 44.25937500034140015, 47.42413220539094709 ) ) ;
#8992 = ORIENTED_EDGE ( 'NONE', *, *, #8453, .T. ) ;
#8993 = CARTESIAN_POINT ( 'NONE',  ( -45.00000000000000000, 262.0000000000000000, -10.00000000000000178 ) ) ;
#8994 = VECTOR ( 'NONE', #8786, 1000.000000000000000 ) ;
#8995 = CARTESIAN_POINT ( 'NONE',  ( 0.000000000000000000, 242.0000000000000284, 0.000000000000000000 ) ) ;
#8996 = CARTESIAN_POINT ( 'NONE',  ( 49.86468353124999453, 28.95937500034139944, -16.20201782572376459 ) ) ;
#8997 = ORIENTED_EDGE ( 'NONE', *, *, #5569, .F. ) ;
#8998 = CARTESIAN_POINT ( 'NONE',  ( 0.000000000000000000, 217.0000000000000284, 45.00000000000000000 ) ) ;
#8999 = DIRECTION ( 'NONE',  ( 0.000000000000000000, 0.000000000000000000, 1.000000000000000000 ) ) ;
#9000 = CARTESIAN_POINT ( 'NONE',  ( 48.20095974065459643, 25.00000000000000000, -12.77318064350110838 ) ) ;
#9001 = CARTESIAN_POINT ( 'NONE',  ( -15.40903463028480580, 32.32187500034139305, 47.42413220539094709 ) ) ;
#9002 = DIRECTION ( 'NONE',  ( 0.000000000000000000, -0.000000000000000000, 1.000000000000000000 ) ) ;
#9003 = CARTESIAN_POINT ( 'NONE',  ( -49.86468353124999453, 25.75937500034139660, -16.20201782572375393 ) ) ;
#9004 = CARTESIAN_POINT ( 'NONE',  ( 7.513064459987437071E-14, 42.50000000000000000, 50.00000000000000000 ) ) ;
#9005 = ADVANCED_FACE ( 'NONE', ( #13946 ), #15784, .T. ) ;
#9006 = CARTESIAN_POINT ( 'NONE',  ( -49.86468353124999453, 31.82187500034139305, -16.20201782572375393 ) ) ;
#9007 = AXIS2_PLACEMENT_3D ( 'NONE', #6333, #5093, #13871 ) ;
#9008 = CARTESIAN_POINT ( 'NONE',  ( 40.45084971874737789, 30.80000000000000071, 29.38926261462365375 ) ) ;
#9009 = EDGE_CURVE ( 'NONE', #9775, #11764, #11229, .T. ) ;
#9010 = CARTESIAN_POINT ( 'NONE',  ( 30.81806926056964002, 38.55937500034140442, 42.41743335407647209 ) ) ;
#9011 = CARTESIAN_POINT ( 'NONE',  ( 49.86468353125001585, 32.82187500034139305, 16.20201782572375038 ) ) ;
#9012 = CARTESIAN_POINT ( 'NONE',  ( -40.45084971874737789, 41.80000000000000426, -29.38926261462365730 ) ) ;
#9013 = ORIENTED_EDGE ( 'NONE', *, *, #12004, .F. ) ;
#9014 = EDGE_CURVE ( 'NONE', #4580, #3492, #16456, .T. ) ;
#9015 = CARTESIAN_POINT ( 'NONE',  ( 15.40903463028482356, 38.45937500034139589, 47.42413220539093999 ) ) ;
#9016 = VERTEX_POINT ( 'NONE', #5258 ) ;
#9017 = VERTEX_POINT ( 'NONE', #16372 ) ;
#9018 = CARTESIAN_POINT ( 'NONE',  ( 30.00000000000001066, 282.0000000000000000, -12.50000000000000000 ) ) ;
#9019 = CARTESIAN_POINT ( 'NONE',  ( 15.40903463028482356, 46.45937500034139589, 47.42413220539093999 ) ) ;
#9020 = AXIS2_PLACEMENT_3D ( 'NONE', #1299, #4904, #6222 ) ;
#9021 = DIRECTION ( 'NONE',  ( 0.000000000000000000, 0.000000000000000000, -1.000000000000000000 ) ) ;
#9022 = CARTESIAN_POINT ( 'NONE',  ( 40.34137639590981195, 27.12187500034139731, -29.30972558990011834 ) ) ;
#9023 = PLANE ( 'NONE',  #10255 ) ;
#9024 = CARTESIAN_POINT ( 'NONE',  ( 49.86468353125001585, 40.82187500034140726, 16.20201782572375038 ) ) ;
#9025 = CARTESIAN_POINT ( 'NONE',  ( 9.631387414534489405E-15, 42.35937500034140157, 52.43083105670540789 ) ) ;
#9026 = DIRECTION ( 'NONE',  ( 0.000000000000000000, 0.000000000000000000, 1.000000000000000000 ) ) ;
#9027 = CARTESIAN_POINT ( 'NONE',  ( -30.90169943749473802, 48.30000000000000426, 42.53254041760200721 ) ) ;
#9028 = CARTESIAN_POINT ( 'NONE',  ( -30.90169943749474868, 25.48125000068279888, -42.53254041760200721 ) ) ;
#9029 = CARTESIAN_POINT ( 'NONE',  ( 17.06320572571393157, 26.42681735030989998, 93.80094291277063689 ) ) ;
#9030 = CIRCLE ( 'NONE', #1846, 47.00000000000000000 ) ;
#9031 = CARTESIAN_POINT ( 'NONE',  ( -49.86468353124999453, 29.82187500034139660, -16.20201782572375393 ) ) ;
#9032 = CYLINDRICAL_SURFACE ( 'NONE', #896, 82.49773270518484480 ) ;
#9033 = VERTEX_POINT ( 'NONE', #8720 ) ;
#9034 = CARTESIAN_POINT ( 'NONE',  ( -40.45084971874737789, 39.58125000068280031, -29.38926261462365730 ) ) ;
#9035 = VERTEX_POINT ( 'NONE', #2400 ) ;
#9036 = CARTESIAN_POINT ( 'NONE',  ( 2.600676159226420495E-13, 31.49999999999999289, -49.99999999999999289 ) ) ;
#9037 = CARTESIAN_POINT ( 'NONE',  ( 14.82166083077715513, 14.52006039870328458, 101.6666710451724214 ) ) ;
#9038 =( BOUNDED_CURVE ( )  B_SPLINE_CURVE ( 2, ( #2368, #6046, #865, #11022, #16092, #9786, #4725, #14831, #3460, #11118, #14996, #10277, #13913 ),
 .UNSPECIFIED., .F., .F. ) 
 B_SPLINE_CURVE_WITH_KNOTS ( ( 3, 2, 2, 2, 2, 2, 3 ),
 ( 0.2833333333333333814, 0.2866666666666666807, 0.2933333333333333348, 0.2999999999999999889, 0.3066666666666666430, 0.3133333333333333526, 0.3166666666666667074 ),
 .UNSPECIFIED. ) 
 CURVE ( )  GEOMETRIC_REPRESENTATION_ITEM ( )  RATIONAL_B_SPLINE_CURVE ( ( 0.9755282581475768211, 0.9755282581475770431, 1.000000000000000000, 0.9510565162951535312, 1.000000000000000000, 0.9510565162951535312, 1.000000000000000000, 0.9510565162951535312, 1.000000000000000000, 0.9510565162951535312, 1.000000000000000000, 0.9755282581475765991, 0.9755282581475768211 ) ) 
 REPRESENTATION_ITEM ( '' )  );
#9039 = CARTESIAN_POINT ( 'NONE',  ( -7.919222016226688865, 23.55125428154684641, -50.00000000000003553 ) ) ;
#9040 = CARTESIAN_POINT ( 'NONE',  ( 30.81806926056962936, 49.22187500034139873, -42.41743335407646498 ) ) ;
#9041 = CARTESIAN_POINT ( 'NONE',  ( 15.40903463028482356, 34.45937500034139589, 47.42413220539093999 ) ) ;
#9042 = DIRECTION ( 'NONE',  ( -1.000000000000000000, 0.000000000000000000, -1.734723475976806848E-16 ) ) ;
#9043 = CARTESIAN_POINT ( 'NONE',  ( 40.34137639590981195, 45.12187500034139731, -29.30972558990011834 ) ) ;
#9044 = APPLICATION_PROTOCOL_DEFINITION ( 'draft international standard', 'automotive_design', 1998, #10998 ) ;
#9045 = CARTESIAN_POINT ( 'NONE',  ( 2.500000000000000000, 247.0000000000000284, -47.99999999999999289 ) ) ;
#9046 = CARTESIAN_POINT ( 'NONE',  ( -1.240322475938754499E-13, 36.28125000068280315, 50.00000000000000000 ) ) ;
#9047 = CARTESIAN_POINT ( 'NONE',  ( -9.289494224341229511, 8.863457290943159705, 102.0000000000000142 ) ) ;
#9048 = ORIENTED_EDGE ( 'NONE', *, *, #10371, .T. ) ;
#9049 = EDGE_CURVE ( 'NONE', #3473, #8435, #5009, .T. ) ;
#9050 = CARTESIAN_POINT ( 'NONE',  ( 30.81806926056964002, 46.62187500034140442, 42.41743335407647209 ) ) ;
#9051 = ORIENTED_EDGE ( 'NONE', *, *, #4907, .F. ) ;
#9052 = FACE_OUTER_BOUND ( 'NONE', #1704, .T. ) ;
#9053 = ORIENTED_EDGE ( 'NONE', *, *, #3497, .F. ) ;
#9054 = ORIENTED_EDGE ( 'NONE', *, *, #7778, .T. ) ;
#9055 = CARTESIAN_POINT ( 'NONE',  ( 49.99999999999999289, 34.88125000068280457, -16.24598481164532160 ) ) ;
#9056 = DIRECTION ( 'NONE',  ( -1.000000000000000000, 0.000000000000000000, 0.000000000000000000 ) ) ;
#9057 = EDGE_CURVE ( 'NONE', #15672, #9777, #9707, .T. ) ;
#9058 = EDGE_CURVE ( 'NONE', #7884, #11917, #10309, .T. ) ;
#9059 = CARTESIAN_POINT ( 'NONE',  ( 15.45084971874737789, 28.60000000000000142, 47.55282581475767500 ) ) ;
#9060 = CARTESIAN_POINT ( 'NONE',  ( -50.00000000000000000, 22.00000000000000355, 0.000000000000000000 ) ) ;
#9061 = CARTESIAN_POINT ( 'NONE',  ( -49.86468353124999453, 47.75937500034139305, -16.20201782572375393 ) ) ;
#9062 = DIRECTION ( 'NONE',  ( 0.000000000000000000, 0.000000000000000000, 1.000000000000000000 ) ) ;
#9063 = CARTESIAN_POINT ( 'NONE',  ( 15.45084971874737789, 48.38125000068280457, 47.55282581475767500 ) ) ;
#9064 = CARTESIAN_POINT ( 'NONE',  ( 24.99999999999999645, 287.0000000000000568, 2.500000000000003109 ) ) ;
#9065 = ADVANCED_FACE ( 'NONE', ( #14034 ), #10061, .F. ) ;
#9066 = SURFACE_STYLE_FILL_AREA ( #13874 ) ;
#9067 = DIRECTION ( 'NONE',  ( 0.000000000000000000, 8.780190904559502465E-17, 1.000000000000000000 ) ) ;
#9068 = CARTESIAN_POINT ( 'NONE',  ( -30.90169943749473802, 38.08125000068280031, 42.53254041760200721 ) ) ;
#9069 = CARTESIAN_POINT ( 'NONE',  ( 1.036604930454412972E-14, 98.25246584726775723, 9.080892972013893782 ) ) ;
#9070 = CARTESIAN_POINT ( 'NONE',  ( -2.500000000000000000, 247.0000000000000284, -47.99999999999999289 ) ) ;
#9071 = FACE_OUTER_BOUND ( 'NONE', #11891, .T. ) ;
#9072 = ORIENTED_EDGE ( 'NONE', *, *, #10150, .F. ) ;
#9073 = CARTESIAN_POINT ( 'NONE',  ( -40.34137639590981195, 40.05937500034140442, 29.30972558990012189 ) ) ;
#9074 = ORIENTED_EDGE ( 'NONE', *, *, #14423, .F. ) ;
#9075 = CARTESIAN_POINT ( 'NONE',  ( 30.90169943749475223, 42.48125000068279888, 42.53254041760199300 ) ) ;
#9076 = CARTESIAN_POINT ( 'NONE',  ( 9.297345850538470396E-15, 92.00000000000001421, -1.969248798088869855E-14 ) ) ;
#9077 = CARTESIAN_POINT ( 'NONE',  ( -49.86468353124999453, 29.95937500034139944, 16.20201782572377525 ) ) ;
#9078 = VERTEX_POINT ( 'NONE', #1314 ) ;
#9079 = DIRECTION ( 'NONE',  ( 0.000000000000000000, 0.000000000000000000, 1.000000000000000000 ) ) ;
#9080 = CARTESIAN_POINT ( 'NONE',  ( 0.000000000000000000, 22.50000000000000000, 101.0000000000000000 ) ) ;
#9081 = CARTESIAN_POINT ( 'NONE',  ( 47.98103867763196462, 25.00000000000000000, -13.57697939761754036 ) ) ;
#9082 = CARTESIAN_POINT ( 'NONE',  ( 9.631387414534489405E-15, 34.42187500034139447, 52.43083105670540789 ) ) ;
#9083 = CARTESIAN_POINT ( 'NONE',  ( 2.600676159226421000E-13, 21.50000000000000000, -49.99999999999999289 ) ) ;
#9084 = CARTESIAN_POINT ( 'NONE',  ( 49.86468353125001585, 22.75937500034139660, 16.20201782572375038 ) ) ;
#9085 = FACE_BOUND ( 'NONE', #14754, .T. ) ;
#9086 = CARTESIAN_POINT ( 'NONE',  ( -30.81806926056963292, 27.62187500034139731, -42.41743335407646498 ) ) ;
#9087 = DIRECTION ( 'NONE',  ( -0.000000000000000000, -1.000000000000000000, -0.000000000000000000 ) ) ;
#9088 = CARTESIAN_POINT ( 'NONE',  ( -15.45084971874737256, 29.60000000000000142, -47.55282581475767500 ) ) ;
#9089 = CARTESIAN_POINT ( 'NONE',  ( 15.40903463028482356, 34.45937500034139589, 47.42413220539093999 ) ) ;
#9090 = CARTESIAN_POINT ( 'NONE',  ( 9.631387414534489405E-15, 30.42187500034139447, 52.43083105670540789 ) ) ;
#9091 = VERTEX_POINT ( 'NONE', #10140 ) ;
#9092 = UNCERTAINTY_MEASURE_WITH_UNIT (LENGTH_MEASURE( 1.000000000000000082E-05 ), #11140, 'distance_accuracy_value', 'NONE');
#9093 = CARTESIAN_POINT ( 'NONE',  ( 30.81806926056962936, 39.15937500034139873, -42.41743335407646498 ) ) ;
#9094 = ORIENTED_EDGE ( 'NONE', *, *, #10483, .F. ) ;
#9095 = VERTEX_POINT ( 'NONE', #2649 ) ;
#9096 = CARTESIAN_POINT ( 'NONE',  ( 25.00000000000000355, 286.6727470533787709, -2.499999999998864020 ) ) ;
#9097 = CARTESIAN_POINT ( 'NONE',  ( 30.81806926056962936, 45.15937500034139873, -42.41743335407647209 ) ) ;
#9098 = DIRECTION ( 'NONE',  ( -0.000000000000000000, -1.000000000000000000, -0.000000000000000000 ) ) ;
#9099 = CARTESIAN_POINT ( 'NONE',  ( 30.81806926056962936, 25.22187500034139873, -42.41743335407647209 ) ) ;
#9100 = LINE ( 'NONE', #5059, #12372 ) ;
#9101 = CARTESIAN_POINT ( 'NONE',  ( 30.81806926056964002, 34.62187500034139731, 42.41743335407647209 ) ) ;
#9102 = CARTESIAN_POINT ( 'NONE',  ( 40.34137639590981195, 41.05937500034139731, -29.30972558990011834 ) ) ;
#9103 = CARTESIAN_POINT ( 'NONE',  ( -12.59082374547745076, 33.16401225666594854, 102.0000000000000142 ) ) ;
#9104 = CARTESIAN_POINT ( 'NONE',  ( -49.86468353124999453, 20.02187500034139589, 16.20201782572377525 ) ) ;
#9105 = EDGE_CURVE ( 'NONE', #5127, #8121, #8887, .T. ) ;
#9106 = CARTESIAN_POINT ( 'NONE',  ( 30.90169943749475578, 24.48125000068280244, 42.53254041760200010 ) ) ;
#9107 = CARTESIAN_POINT ( 'NONE',  ( 7.778087436843963864, 38.21832046643818614, 92.94215756931615147 ) ) ;
#9108 = CARTESIAN_POINT ( 'NONE',  ( -49.86468353124999453, 30.02187500034139234, 16.20201782572377525 ) ) ;
#9109 = CARTESIAN_POINT ( 'NONE',  ( -40.45084971874737789, 27.80000000000000071, -29.38926261462365730 ) ) ;
#9110 = VERTEX_POINT ( 'NONE', #6403 ) ;
#9111 = CARTESIAN_POINT ( 'NONE',  ( 40.45084971874737079, 34.98125000068279888, -29.38926261462366440 ) ) ;
#9112 = AXIS2_PLACEMENT_3D ( 'NONE', #15796, #574, #14217 ) ;
#9113 = ORIENTED_EDGE ( 'NONE', *, *, #815, .T. ) ;
#9114 = CARTESIAN_POINT ( 'NONE',  ( -3.111920190527341144E-15, 25.28125000068279604, -50.00000000000000000 ) ) ;
#9115 = PLANE ( 'NONE',  #8923 ) ;
#9116 = CARTESIAN_POINT ( 'NONE',  ( 2.600676159226420495E-13, 23.50000000000000000, -49.99999999999999289 ) ) ;
#9117 = CARTESIAN_POINT ( 'NONE',  ( -49.86468353125000164, 47.92187500034139447, 0.000000000000000000 ) ) ;
#9118 = CARTESIAN_POINT ( 'NONE',  ( 49.86468353125001585, 24.75937500034140015, 16.20201782572375038 ) ) ;
#9119 = CARTESIAN_POINT ( 'NONE',  ( 10.69075041230586365, 8.636095224584757091, 102.0000000000000142 ) ) ;
#9120 = CARTESIAN_POINT ( 'NONE',  ( -15.40903463028480580, 48.32187500034140015, 47.42413220539094709 ) ) ;
#9121 = DIRECTION ( 'NONE',  ( 0.000000000000000000, 0.000000000000000000, 1.000000000000000000 ) ) ;
#9122 = CARTESIAN_POINT ( 'NONE',  ( 6.725310538855729270, 29.22831317314791733, 101.0000000000000000 ) ) ;
#9123 = VECTOR ( 'NONE', #8401, 1000.000000000000000 ) ;
#9124 = CARTESIAN_POINT ( 'NONE',  ( 49.86468353124999453, 49.02187500034140299, -16.20201782572376459 ) ) ;
#9125 = CARTESIAN_POINT ( 'NONE',  ( 40.45084971874737789, 28.58125000068280031, 29.38926261462365375 ) ) ;
#9126 = ORIENTED_EDGE ( 'NONE', *, *, #10357, .T. ) ;
#9127 = CARTESIAN_POINT ( 'NONE',  ( 40.34137639590981195, 47.12187500034140442, -29.30972558990011834 ) ) ;
#9128 = ORIENTED_EDGE ( 'NONE', *, *, #6497, .T. ) ;
#9129 = CYLINDRICAL_SURFACE ( 'NONE', #6825, 2.000000000000001776 ) ;
#9130 = ORIENTED_EDGE ( 'NONE', *, *, #1049, .T. ) ;
#9131 = ORIENTED_EDGE ( 'NONE', *, *, #4713, .F. ) ;
#9132 =( BOUNDED_CURVE ( )  B_SPLINE_CURVE ( 2, ( #5146, #10202, #13926, #120, #2545, #8701, #13767, #5234, #16265, #3962, #2379, #11286, #9036 ),
 .UNSPECIFIED., .F., .F. ) 
 B_SPLINE_CURVE_WITH_KNOTS ( ( 3, 2, 2, 2, 2, 2, 3 ),
 ( 0.5833333333333333703, 0.5866666666666666696, 0.5933333333333333792, 0.5999999999999999778, 0.6066666666666666874, 0.6133333333333332860, 0.6166666666666666963 ),
 .UNSPECIFIED. ) 
 CURVE ( )  GEOMETRIC_REPRESENTATION_ITEM ( )  RATIONAL_B_SPLINE_CURVE ( ( 0.9755282581475768211, 0.9755282581475771542, 1.000000000000000000, 0.9510565162951535312, 1.000000000000000000, 0.9510565162951535312, 1.000000000000000000, 0.9510565162951535312, 1.000000000000000000, 0.9510565162951535312, 1.000000000000000000, 0.9755282581475763770, 0.9755282581475768211 ) ) 
 REPRESENTATION_ITEM ( '' )  );
#9133 = EDGE_CURVE ( 'NONE', #10385, #11502, #6521, .T. ) ;
#9134 = CARTESIAN_POINT ( 'NONE',  ( -30.90169943749473447, 44.08125000068279320, 42.53254041760200721 ) ) ;
#9135 = DIRECTION ( 'NONE',  ( -0.000000000000000000, 1.000000000000000000, -0.000000000000000000 ) ) ;
#9136 = AXIS2_PLACEMENT_3D ( 'NONE', #558, #15372, #9067 ) ;
#9137 = CARTESIAN_POINT ( 'NONE',  ( 49.99999999999999289, 27.10000000000000497, -16.24598481164532160 ) ) ;
#9138 = CARTESIAN_POINT ( 'NONE',  ( 49.86468353124999453, 48.95937500034140299, -16.20201782572376459 ) ) ;
#9139 = CARTESIAN_POINT ( 'NONE',  ( -49.99999999999999289, 31.88125000068280102, 16.24598481164533226 ) ) ;
#9140 = FACE_OUTER_BOUND ( 'NONE', #13219, .T. ) ;
#9141 = EDGE_CURVE ( 'NONE', #15007, #11588, #12629, .T. ) ;
#9142 = CARTESIAN_POINT ( 'NONE',  ( 30.81806926056964002, 22.62187500034139731, 42.41743335407647209 ) ) ;
#9143 = CARTESIAN_POINT ( 'NONE',  ( -10.09851121871618140, 9.451242543235633065, 102.0000000000000142 ) ) ;
#9144 = CARTESIAN_POINT ( 'NONE',  ( -40.45084971874737789, 37.58125000068280031, -29.38926261462365730 ) ) ;
#9145 = CARTESIAN_POINT ( 'NONE',  ( -30.90169943749474513, 37.48125000068279888, -42.53254041760200721 ) ) ;
#9146 = CARTESIAN_POINT ( 'NONE',  ( -2.445080149700054274E-14, 46.28125000068280315, 50.00000000000000000 ) ) ;
#9147 = CARTESIAN_POINT ( 'NONE',  ( 25.00000000000000000, 312.0000000000000568, -2.499999999999997780 ) ) ;
#9148 = EDGE_CURVE ( 'NONE', #13843, #2741, #551, .T. ) ;
#9149 = PRODUCT_DEFINITION ( 'UNKNOWN', '', #947, #2767 ) ;
#9150 = ORIENTED_EDGE ( 'NONE', *, *, #16075, .T. ) ;
#9151 = AXIS2_PLACEMENT_3D ( 'NONE', #14953, #16376, #5914 ) ;
#9152 = CARTESIAN_POINT ( 'NONE',  ( -40.34137639590981195, 36.05937500034139731, 29.30972558990012189 ) ) ;
#9153 = VERTEX_POINT ( 'NONE', #1644 ) ;
#9154 = DIRECTION ( 'NONE',  ( 0.000000000000000000, -0.000000000000000000, 1.000000000000000000 ) ) ;
#9155 = CYLINDRICAL_SURFACE ( 'NONE', #16116, 50.00000000000000000 ) ;
#9156 = CARTESIAN_POINT ( 'NONE',  ( -30.81806926056962226, 24.15937500034139873, 42.41743335407647919 ) ) ;
#9157 = VERTEX_POINT ( 'NONE', #388 ) ;
#9158 = LINE ( 'NONE', #8998, #8922 ) ;
#9159 = CARTESIAN_POINT ( 'NONE',  ( -7.790398555160043870, 38.21309231270640794, 92.94217575349884441 ) ) ;
#9160 = CARTESIAN_POINT ( 'NONE',  ( 7.735767786613922123E-15, 54.00000000000000711, -63.16733765196516970 ) ) ;
#9161 = CARTESIAN_POINT ( 'NONE',  ( 30.81806926056964002, 28.62187500034139731, 42.41743335407646498 ) ) ;
#9162 = VECTOR ( 'NONE', #9571, 1000.000000000000000 ) ;
#9163 = ADVANCED_FACE ( 'NONE', ( #309 ), #15525, .T. ) ;
#9164 = CARTESIAN_POINT ( 'NONE',  ( -40.45084971874737789, 29.58125000068279675, -29.38926261462365730 ) ) ;
#9165 = PLANE ( 'NONE',  #14411 ) ;
#9166 = CARTESIAN_POINT ( 'NONE',  ( -47.79496856443377339, 20.00000000000000355, 14.21716018044757668 ) ) ;
#9167 = CARTESIAN_POINT ( 'NONE',  ( -40.34137639590981195, 32.12187500034140442, 29.30972558990012189 ) ) ;
#9168 = CARTESIAN_POINT ( 'NONE',  ( -15.45084971874736368, 22.39999999999999858, 47.55282581475768211 ) ) ;
#9169 = CARTESIAN_POINT ( 'NONE',  ( -15.45084971874737256, 31.60000000000000142, -47.55282581475767500 ) ) ;
#9170 = CARTESIAN_POINT ( 'NONE',  ( -3.210462471511496205E-15, 33.35937500034140157, -52.43083105670540789 ) ) ;
#9171 = CARTESIAN_POINT ( 'NONE',  ( -30.81806926056962226, 28.22187500034139873, 42.41743335407647919 ) ) ;
#9172 = CARTESIAN_POINT ( 'NONE',  ( -2.464234863135557063, 13.31155363843772932, 101.0000000000000000 ) ) ;
#9173 = ORIENTED_EDGE ( 'NONE', *, *, #13712, .T. ) ;
#9174 = VECTOR ( 'NONE', #16348, 999.9999999999998863 ) ;
#9175 = EDGE_CURVE ( 'NONE', #14909, #15954, #7315, .T. ) ;
#9176 = CARTESIAN_POINT ( 'NONE',  ( 15.40903463028482356, 30.45937500034139589, 47.42413220539093999 ) ) ;
#9177 = ORIENTED_EDGE ( 'NONE', *, *, #8538, .F. ) ;
#9178 =( GEOMETRIC_REPRESENTATION_CONTEXT ( 3 ) GLOBAL_UNCERTAINTY_ASSIGNED_CONTEXT ( ( #6615 ) ) GLOBAL_UNIT_ASSIGNED_CONTEXT ( ( #12209, #3147, #5897 ) ) REPRESENTATION_CONTEXT ( 'NONE', 'WORKASPACE' ) );
#9179 = CARTESIAN_POINT ( 'NONE',  ( 26.78441608355291947, 282.9883952696292226, -9.284416083551356280 ) ) ;
#9180 = CARTESIAN_POINT ( 'NONE',  ( 15.40903463028481113, 49.25937500034139305, -47.42413220539094709 ) ) ;
#9181 = CARTESIAN_POINT ( 'NONE',  ( -7.919222016226752814, 37.55125428154683931, -50.00000000000000711 ) ) ;
#9182 = CARTESIAN_POINT ( 'NONE',  ( 27.78424396843206878, 282.5058351977235134, 8.068487936863856902 ) ) ;
#9183 = CARTESIAN_POINT ( 'NONE',  ( -2.518620260143848100, 35.01862026014384099, -40.00000000000000711 ) ) ;
#9184 = CARTESIAN_POINT ( 'NONE',  ( -30.81806926056963292, 35.62187500034140442, -42.41743335407647209 ) ) ;
#9185 = CARTESIAN_POINT ( 'NONE',  ( 30.81806926056962936, 43.15937500034139873, -42.41743335407646498 ) ) ;
#9186 = AXIS2_PLACEMENT_3D ( 'NONE', #11358, #1189, #5135 ) ;
#9187 = LINE ( 'NONE', #5547, #15558 ) ;
#9188 = AXIS2_PLACEMENT_3D ( 'NONE', #5834, #12398, #3581 ) ;
#9189 = CARTESIAN_POINT ( 'NONE',  ( 30.90169943749475578, 40.69999999999999574, 42.53254041760200010 ) ) ;
#9190 = PRODUCT_DEFINITION_SHAPE ( 'NONE', 'NONE',  #4279 ) ;
#9191 = CARTESIAN_POINT ( 'NONE',  ( -3.210462471511496205E-15, 49.35937500034138736, -52.43083105670540789 ) ) ;
#9192 = CARTESIAN_POINT ( 'NONE',  ( 6.190300238984888459, 38.87860627667793523, 92.94022342448253937 ) ) ;
#9193 =( GEOMETRIC_REPRESENTATION_CONTEXT ( 3 ) GLOBAL_UNCERTAINTY_ASSIGNED_CONTEXT ( ( #265 ) ) GLOBAL_UNIT_ASSIGNED_CONTEXT ( ( #1967, #3484, #2636 ) ) REPRESENTATION_CONTEXT ( 'NONE', 'WORKASPACE' ) );
#9194 = ADVANCED_BREP_SHAPE_REPRESENTATION ( '', ( #14597, #15812 ), #1738 ) ;
#9195 = CARTESIAN_POINT ( 'NONE',  ( 9.631387414534489405E-15, 26.42187500034139447, 52.43083105670540789 ) ) ;
#9196 = EDGE_CURVE ( 'NONE', #13613, #15272, #6822, .T. ) ;
#9197 = DIRECTION ( 'NONE',  ( 0.000000000000000000, 1.000000000000000000, 0.000000000000000000 ) ) ;
#9198 = CIRCLE ( 'NONE', #12651, 40.00000000000000000 ) ;
#9199 = ORIENTED_EDGE ( 'NONE', *, *, #15522, .T. ) ;
#9200 = AXIS2_PLACEMENT_3D ( 'NONE', #15140, #6352, #11418 ) ;
#9201 = CONICAL_SURFACE ( 'NONE', #12106, 16.50000000000000711, 0.7853981633974447263 ) ;
#9202 = CARTESIAN_POINT ( 'NONE',  ( -49.99999999999999289, 35.68125000068278752, -16.24598481164531449 ) ) ;
#9203 = ORIENTED_EDGE ( 'NONE', *, *, #5236, .T. ) ;
#9204 = DIRECTION ( 'NONE',  ( -0.000000000000000000, -0.000000000000000000, -1.000000000000000000 ) ) ;
#9205 = CARTESIAN_POINT ( 'NONE',  ( 7.164845293663816506, 37.36320934111687109, 102.0000000000000142 ) ) ;
#9206 = CARTESIAN_POINT ( 'NONE',  ( 50.00000000000000000, 30.78125000068279959, -6.123233995736766085E-15 ) ) ;
#9207 = CARTESIAN_POINT ( 'NONE',  ( 49.86468353125001585, 46.82187500034139305, 16.20201782572375038 ) ) ;
#9208 =( BOUNDED_CURVE ( )  B_SPLINE_CURVE ( 3, ( #2264, #7274, #14645, #9849 ),
 .UNSPECIFIED., .F., .T. ) 
 B_SPLINE_CURVE_WITH_KNOTS ( ( 4, 4 ),
 ( 4.712388980384689674, 6.283185307179586232 ),
 .UNSPECIFIED. ) 
 CURVE ( )  GEOMETRIC_REPRESENTATION_ITEM ( )  RATIONAL_B_SPLINE_CURVE ( ( 1.000000000000000000, 0.8047378541243649375, 0.8047378541243649375, 1.000000000000000000 ) ) 
 REPRESENTATION_ITEM ( '' )  );
#9209 = CARTESIAN_POINT ( 'NONE',  ( -49.86468353124999453, 21.95937500034138878, 16.20201782572377525 ) ) ;
#9210 = CYLINDRICAL_SURFACE ( 'NONE', #12640, 50.00000000000000000 ) ;
#9211 = CARTESIAN_POINT ( 'NONE',  ( -15.40903463028480580, 42.32187500034139305, 47.42413220539094709 ) ) ;
#9212 = VECTOR ( 'NONE', #6354, 1000.000000000000000 ) ;
#9213 = APPLICATION_PROTOCOL_DEFINITION ( 'draft international standard', 'automotive_design', 1998, #3244 ) ;
#9215 = DIRECTION ( 'NONE',  ( -0.000000000000000000, -1.000000000000000000, -0.000000000000000000 ) ) ;
#9214 = VECTOR ( 'NONE', #11800, 1000.000000000000227 ) ;
#9216 = CARTESIAN_POINT ( 'NONE',  ( 49.86468353125001585, 46.82187500034139305, 16.20201782572375038 ) ) ;
#9217 = CARTESIAN_POINT ( 'NONE',  ( -17.35186893731094671, 20.17349094513186358, 101.0000000000000000 ) ) ;
#9218 = EDGE_LOOP ( 'NONE', ( #14590, #1184, #1455, #6255 ) ) ;
#9219 = CARTESIAN_POINT ( 'NONE',  ( -40.34137639590981905, 45.72187500034139873, -29.30972558990011478 ) ) ;
#9220 = ORIENTED_EDGE ( 'NONE', *, *, #1334, .T. ) ;
#9221 = CARTESIAN_POINT ( 'NONE',  ( -45.58196769024076644, 258.6644603543468861, -10.00000000000000178 ) ) ;
#9222 = EDGE_LOOP ( 'NONE', ( #4598, #6917, #7703, #13596 ) ) ;
#9223 = ORIENTED_EDGE ( 'NONE', *, *, #5772, .T. ) ;
#9224 = AXIS2_PLACEMENT_3D ( 'NONE', #10421, #15475, #14225 ) ;
#9225 = CARTESIAN_POINT ( 'NONE',  ( -7.919222016226838967, 44.22999571913595673, 49.99999999999999289 ) ) ;
#9226 = DIRECTION ( 'NONE',  ( 0.000000000000000000, -0.7071067811865487940, 0.7071067811865463515 ) ) ;
#9227 = AXIS2_PLACEMENT_3D ( 'NONE', #16016, #8459, #14761 ) ;
#9228 = SURFACE_STYLE_USAGE ( .BOTH. , #10390 ) ;
#9229 = CARTESIAN_POINT ( 'NONE',  ( -49.99999999999999289, 24.10000000000000142, 16.24598481164533226 ) ) ;
#9230 = CARTESIAN_POINT ( 'NONE',  ( -49.86468353125000164, 41.85937500034139447, 0.000000000000000000 ) ) ;
#9231 = CARTESIAN_POINT ( 'NONE',  ( 2.600676159226420495E-13, 31.28125000068279604, -49.99999999999999289 ) ) ;
#9232 = DIRECTION ( 'NONE',  ( 0.000000000000000000, 0.000000000000000000, -1.000000000000000000 ) ) ;
#9233 = CARTESIAN_POINT ( 'NONE',  ( -7.919222016226816763, 45.55125428154684641, -49.99999999999999289 ) ) ;
#9234 = AXIS2_PLACEMENT_3D ( 'NONE', #13653, #7112, #2261 ) ;
#9235 = CARTESIAN_POINT ( 'NONE',  ( -10.49054022437444900, 8.911660907547297228, 101.3333374614808662 ) ) ;
#9236 = CARTESIAN_POINT ( 'NONE',  ( -49.99999999999999289, 41.88125000068279746, 16.24598481164533226 ) ) ;
#9237 = CARTESIAN_POINT ( 'NONE',  ( 1.293669679204937499E-13, 39.50000000000000711, -50.00000000000000000 ) ) ;
#9238 = CARTESIAN_POINT ( 'NONE',  ( 30.90169943749475223, 22.48125000068279533, 42.53254041760199300 ) ) ;
#9239 = DIRECTION ( 'NONE',  ( -0.9135454576426059736, 0.4067366430757887730, 0.000000000000000000 ) ) ;
#9240 = ORIENTED_EDGE ( 'NONE', *, *, #2139, .F. ) ;
#9241 =( BOUNDED_CURVE ( )  B_SPLINE_CURVE ( 2, ( #5310, #10360, #607, #15593, #6797, #13335, #7944, #13096, #452, #4214, #11847, #1701, #5553 ),
 .UNSPECIFIED., .F., .F. ) 
 B_SPLINE_CURVE_WITH_KNOTS ( ( 3, 2, 2, 2, 2, 2, 3 ),
 ( 0.7166666666666666741, 0.7199999999999999734, 0.7266666666666666829, 0.7333333333333332815, 0.7399999999999999911, 0.7466666666666667007, 0.7500000000000000000 ),
 .UNSPECIFIED. ) 
 CURVE ( )  GEOMETRIC_REPRESENTATION_ITEM ( )  RATIONAL_B_SPLINE_CURVE ( ( 0.9755282581475768211, 0.9755282581475768211, 1.000000000000000000, 0.9510565162951535312, 1.000000000000000000, 0.9510565162951535312, 1.000000000000000000, 0.9510565162951535312, 1.000000000000000000, 0.9510565162951535312, 1.000000000000000000, 0.9755282581475768211, 0.9755282581475768211 ) ) 
 REPRESENTATION_ITEM ( '' )  );
#9242 = CARTESIAN_POINT ( 'NONE',  ( -30.81806926056962226, 38.15937500034138452, 42.41743335407647919 ) ) ;
#9243 = EDGE_LOOP ( 'NONE', ( #4575, #13546, #5272, #10443 ) ) ;
#9244 = ORIENTED_EDGE ( 'NONE', *, *, #2520, .F. ) ;
#9245 = CARTESIAN_POINT ( 'NONE',  ( 0.000000000000000000, 20.00000000000000355, 0.000000000000000000 ) ) ;
#9246 = CARTESIAN_POINT ( 'NONE',  ( 0.000000000000000000, 20.00000000000000355, 50.00000000000000000 ) ) ;
#9247 = CARTESIAN_POINT ( 'NONE',  ( 7.347880794884119933E-15, 50.00000000000000000, 60.00000000000000711 ) ) ;
#9248 = EDGE_LOOP ( 'NONE', ( #5179, #14238, #8366, #1389 ) ) ;
#9249 = CARTESIAN_POINT ( 'NONE',  ( -7.919222016226802552, 47.55125428154684641, -50.00000000000000000 ) ) ;
#9250 = CARTESIAN_POINT ( 'NONE',  ( 30.90169943749475223, 34.70000000000000284, 42.53254041760199300 ) ) ;
#9251 = CYLINDRICAL_SURFACE ( 'NONE', #5414, 50.00000000000000000 ) ;
#9252 = CARTESIAN_POINT ( 'NONE',  ( 49.86468353125001585, 28.82187500034139305, 16.20201782572375038 ) ) ;
#9253 = CARTESIAN_POINT ( 'NONE',  ( -24.78626291527390890, 25.00000000000000355, 5.650101528493965297 ) ) ;
#9254 = CARTESIAN_POINT ( 'NONE',  ( 15.72133679436987386, 14.79214933101786222, 96.11488922061346329 ) ) ;
#9255 = CARTESIAN_POINT ( 'NONE',  ( -46.50201513659311559, 20.00000000000000355, 18.00136805656113026 ) ) ;
#9256 = CARTESIAN_POINT ( 'NONE',  ( -30.81806926056962226, 28.22187500034139873, 42.41743335407647209 ) ) ;
#9257 = CARTESIAN_POINT ( 'NONE',  ( 1.293669679204937499E-13, 41.50000000000000000, -50.00000000000000000 ) ) ;
#9258 = CARTESIAN_POINT ( 'NONE',  ( 15.45084971874736723, 37.40000000000000568, -47.55282581475768211 ) ) ;
#9259 = CARTESIAN_POINT ( 'NONE',  ( -15.40903463028480580, 32.25937500034140015, 47.42413220539094709 ) ) ;
#9260 = CARTESIAN_POINT ( 'NONE',  ( -1.486087262401750042, 13.10364194761997503, 101.0000000000000000 ) ) ;
#9261 = ORIENTED_EDGE ( 'NONE', *, *, #2391, .T. ) ;
#9262 = EDGE_CURVE ( 'NONE', #8059, #7640, #13118, .T. ) ;
#9263 = CARTESIAN_POINT ( 'NONE',  ( 30.81806926056964002, 30.55937500034139731, 42.41743335407646498 ) ) ;
#9264 = VERTEX_POINT ( 'NONE', #15614 ) ;
#9265 = FACE_OUTER_BOUND ( 'NONE', #8451, .T. ) ;
#9266 = CARTESIAN_POINT ( 'NONE',  ( -3.210462471511496205E-15, 43.35937500034138736, -52.43083105670540789 ) ) ;
#9267 = CARTESIAN_POINT ( 'NONE',  ( -15.45084971874737256, 37.60000000000000142, -47.55282581475767500 ) ) ;
#9268 = CARTESIAN_POINT ( 'NONE',  ( 0.000000000000000000, 25.00000000000000000, 0.000000000000000000 ) ) ;
#9269 = EDGE_CURVE ( 'NONE', #1639, #3492, #3600, .T. ) ;
#9270 = EDGE_CURVE ( 'NONE', #13515, #6698, #9382, .T. ) ;
#9271 = CARTESIAN_POINT ( 'NONE',  ( -28.38892170791837799, 282.2553694771631854, 9.277843415834363228 ) ) ;
#9272 = VECTOR ( 'NONE', #14285, 1000.000000000000000 ) ;
#9273 = CARTESIAN_POINT ( 'NONE',  ( -30.81806926056962226, 34.22187500034139873, 42.41743335407647919 ) ) ;
#9274 = CARTESIAN_POINT ( 'NONE',  ( -49.86468353124999453, 33.75937500034140015, -16.20201782572375393 ) ) ;
#9275 = DIRECTION ( 'NONE',  ( 0.000000000000000000, 0.000000000000000000, 1.000000000000000000 ) ) ;
#9276 = CARTESIAN_POINT ( 'NONE',  ( 49.99999999999999289, 39.10000000000000853, -16.24598481164532160 ) ) ;
#9277 = EDGE_CURVE ( 'NONE', #8192, #11778, #1735, .T. ) ;
#9278 = CARTESIAN_POINT ( 'NONE',  ( 9.631387414534489405E-15, 48.35937500034140157, 52.43083105670540789 ) ) ;
#9279 = CARTESIAN_POINT ( 'NONE',  ( 30.81806926056962936, 43.22187500034140584, -42.41743335407647209 ) ) ;
#9280 = CARTESIAN_POINT ( 'NONE',  ( -15.40903463028481646, 29.52187500034139589, -47.42413220539093999 ) ) ;
#9281 = COLOUR_RGB ( '', 0.31764706, 0.68627451, 0.89019608) ;
#9282 = CARTESIAN_POINT ( 'NONE',  ( 40.34137639590981195, 47.05937500034140442, -29.30972558990011834 ) ) ;
#9283 = ORIENTED_EDGE ( 'NONE', *, *, #7135, .F. ) ;
#9284 = CARTESIAN_POINT ( 'NONE',  ( 49.99999999999999289, 28.88125000068279391, -16.24598481164532160 ) ) ;
#9285 = ORIENTED_EDGE ( 'NONE', *, *, #7538, .T. ) ;
#9286 = DIRECTION ( 'NONE',  ( 0.8660254037844363761, 0.5000000000000041078, 0.000000000000000000 ) ) ;
#9287 = FACE_OUTER_BOUND ( 'NONE', #16029, .T. ) ;
#9288 = CYLINDRICAL_SURFACE ( 'NONE', #8640, 45.00000000000000000 ) ;
#9289 = CARTESIAN_POINT ( 'NONE',  ( 40.34137639590981195, 45.12187500034139731, -29.30972558990011834 ) ) ;
#9290 = CARTESIAN_POINT ( 'NONE',  ( -49.86468353125000164, 25.85937500034139802, 0.000000000000000000 ) ) ;
#9291 = EDGE_CURVE ( 'NONE', #9644, #1716, #9464, .T. ) ;
#9292 = CARTESIAN_POINT ( 'NONE',  ( 0.000000000000000000, 247.0000000000000284, 0.000000000000000000 ) ) ;
#9293 = CARTESIAN_POINT ( 'NONE',  ( 15.40903463028481113, 39.32187500034140015, -47.42413220539094709 ) ) ;
#9294 = AXIS2_PLACEMENT_3D ( 'NONE', #7889, #5259, #15366 ) ;
#9295 = APPLICATION_PROTOCOL_DEFINITION ( 'draft international standard', 'automotive_design', 1998, #2269 ) ;
#9296 = CARTESIAN_POINT ( 'NONE',  ( 15.45084971874736723, 35.18125000068280173, -47.55282581475768211 ) ) ;
#9297 = ADVANCED_FACE ( 'NONE', ( #1724 ), #4396, .F. ) ;
#9298 = CARTESIAN_POINT ( 'NONE',  ( -40.34137639590981905, 45.72187500034139873, -29.30972558990011478 ) ) ;
#9299 = CARTESIAN_POINT ( 'NONE',  ( 7.919222016226822092, 28.33250428222963890, 49.99999999999999289 ) ) ;
#9300 = ORIENTED_EDGE ( 'NONE', *, *, #5033, .T. ) ;
#9301 = CARTESIAN_POINT ( 'NONE',  ( 49.86468353124999453, 49.02187500034140299, -16.20201782572376459 ) ) ;
#9302 = ORIENTED_EDGE ( 'NONE', *, *, #1781, .F. ) ;
#9303 = CARTESIAN_POINT ( 'NONE',  ( -20.00000000000000355, 284.0710678118655323, 7.500000000000000000 ) ) ;
#9304 = ORIENTED_EDGE ( 'NONE', *, *, #9058, .F. ) ;
#9305 = CARTESIAN_POINT ( 'NONE',  ( -15.45084971874736368, 44.18125000068280173, 47.55282581475768211 ) ) ;
#9306 = DIRECTION ( 'NONE',  ( 1.000000000000000000, 0.000000000000000000, 0.000000000000000000 ) ) ;
#9307 = CARTESIAN_POINT ( 'NONE',  ( -25.00000000000000355, 307.0000000000000568, 2.500000000000001332 ) ) ;
#9308 = CARTESIAN_POINT ( 'NONE',  ( 30.90169943749474157, 25.30000000000000071, -42.53254041760200721 ) ) ;
#9309 = CARTESIAN_POINT ( 'NONE',  ( 30.81806926056964002, 44.55937500034139020, 42.41743335407647209 ) ) ;
#9310 = FACE_OUTER_BOUND ( 'NONE', #5426, .T. ) ;
#9311 = DIRECTION ( 'NONE',  ( 0.000000000000000000, 1.000000000000000000, 0.000000000000000000 ) ) ;
#9312 = FACE_OUTER_BOUND ( 'NONE', #9482, .T. ) ;
#9313 = FACE_OUTER_BOUND ( 'NONE', #5967, .T. ) ;
#9314 = CARTESIAN_POINT ( 'NONE',  ( 40.45084971874737079, 30.98125000068279888, -29.38926261462366440 ) ) ;
#9315 = CARTESIAN_POINT ( 'NONE',  ( 0.000000000000000000, 261.9999999999999432, 49.99999999999999289 ) ) ;
#9316 = EDGE_CURVE ( 'NONE', #15483, #761, #3140, .T. ) ;
#9317 = CARTESIAN_POINT ( 'NONE',  ( 49.99999999999999289, 20.88125000068279746, -16.24598481164532160 ) ) ;
#9318 = EDGE_CURVE ( 'NONE', #14633, #4499, #5471, .T. ) ;
#9319 = CYLINDRICAL_SURFACE ( 'NONE', #1655, 79.49773270518484480 ) ;
#9320 = ORIENTED_EDGE ( 'NONE', *, *, #1205, .T. ) ;
#9321 = CARTESIAN_POINT ( 'NONE',  ( -49.86468353125000164, 37.85937500034139447, 0.000000000000000000 ) ) ;
#9322 = ORIENTED_EDGE ( 'NONE', *, *, #11292, .F. ) ;
#9323 = ORIENTED_EDGE ( 'NONE', *, *, #9772, .T. ) ;
#9324 = FACE_OUTER_BOUND ( 'NONE', #3982, .T. ) ;
#9325 = DIRECTION ( 'NONE',  ( 0.000000000000000000, 0.000000000000000000, 1.000000000000000000 ) ) ;
#9326 = CARTESIAN_POINT ( 'NONE',  ( -49.86468353125000164, 23.85937500034139447, 0.000000000000000000 ) ) ;
#9327 = ORIENTED_EDGE ( 'NONE', *, *, #13339, .F. ) ;
#9328 = DIRECTION ( 'NONE',  ( -0.000000000000000000, 1.000000000000000000, -0.000000000000000000 ) ) ;
#9329 = CARTESIAN_POINT ( 'NONE',  ( 1.088435401685436854E-14, 280.0000000000000000, -88.87749532708107836 ) ) ;
#9330 = DIRECTION ( 'NONE',  ( 1.000000000000000000, -0.000000000000000000, 1.224646799147353207E-16 ) ) ;
#9331 = CARTESIAN_POINT ( 'NONE',  ( 49.86468353124999453, 27.02187500034139944, -16.20201782572376104 ) ) ;
#9332 = CARTESIAN_POINT ( 'NONE',  ( 1.293669679204937499E-13, 37.28125000068280315, -50.00000000000000000 ) ) ;
#9333 = CARTESIAN_POINT ( 'NONE',  ( 14.27695618825629431, 12.36406312199577506, 96.77295768394273523 ) ) ;
#9334 = DIRECTION ( 'NONE',  ( -0.000000000000000000, 0.000000000000000000, 1.000000000000000000 ) ) ;
#9335 = CARTESIAN_POINT ( 'NONE',  ( 15.40903463028482356, 26.52187500034139589, 47.42413220539093999 ) ) ;
#9336 =( BOUNDED_CURVE ( )  B_SPLINE_CURVE ( 2, ( #397, #5506, #15536, #4250, #7898, #10398, #14290, #6834, #5584, #9145, #15455, #2911, #319 ),
 .UNSPECIFIED., .F., .F. ) 
 B_SPLINE_CURVE_WITH_KNOTS ( ( 3, 2, 2, 2, 2, 2, 3 ),
 ( 0.3833333333333333592, 0.3866666666666666585, 0.3933333333333333126, 0.4000000000000000222, 0.4066666666666666763, 0.4133333333333333304, 0.4166666666666666852 ),
 .UNSPECIFIED. ) 
 CURVE ( )  GEOMETRIC_REPRESENTATION_ITEM ( )  RATIONAL_B_SPLINE_CURVE ( ( 0.9755282581475768211, 0.9755282581475770431, 1.000000000000000000, 0.9510565162951535312, 1.000000000000000000, 0.9510565162951535312, 1.000000000000000000, 0.9510565162951535312, 1.000000000000000000, 0.9510565162951535312, 1.000000000000000000, 0.9755282581475765991, 0.9755282581475768211 ) ) 
 REPRESENTATION_ITEM ( '' )  );
#9337 = CARTESIAN_POINT ( 'NONE',  ( -5.000000000000000000, 107.2206331336081320, -16.63484669598115673 ) ) ;
#9338 = CARTESIAN_POINT ( 'NONE',  ( -49.99999999999999289, 34.10000000000000853, 16.24598481164533226 ) ) ;
#9339 = CARTESIAN_POINT ( 'NONE',  ( 15.40903463028481113, 31.25937500034140015, -47.42413220539094709 ) ) ;
#9340 = CARTESIAN_POINT ( 'NONE',  ( 12.59082374547730332, 33.16401225666611197, 102.0000000000000142 ) ) ;
#9341 = ORIENTED_EDGE ( 'NONE', *, *, #3535, .F. ) ;
#9342 = CARTESIAN_POINT ( 'NONE',  ( 49.86468353125001585, 30.75937500034139305, 16.20201782572375038 ) ) ;
#9343 = ORIENTED_EDGE ( 'NONE', *, *, #9912, .F. ) ;
#9344 = CARTESIAN_POINT ( 'NONE',  ( -2.547328955960238000E-13, 22.28125000068279604, 49.99999999999999289 ) ) ;
#9345 = CARTESIAN_POINT ( 'NONE',  ( 40.34137639590981905, 42.65937500034139873, 29.30972558990010768 ) ) ;
#9346 = LINE ( 'NONE', #4028, #9945 ) ;
#9347 = CARTESIAN_POINT ( 'NONE',  ( 26.78441608355448977, 282.9883952696292795, 9.284416083549791310 ) ) ;
#9348 = CARTESIAN_POINT ( 'NONE',  ( -25.00000020635302889, 287.0011902442391261, 7.499999664676339606 ) ) ;
#9349 = CARTESIAN_POINT ( 'NONE',  ( 40.34137639590981195, 37.12187500034139731, -29.30972558990011834 ) ) ;
#9350 = CARTESIAN_POINT ( 'NONE',  ( -30.81806926056963292, 33.55937500034139020, -42.41743335407646498 ) ) ;
#9351 = DIRECTION ( 'NONE',  ( 0.8090169943749426773, 0.5877852522924797984, 0.000000000000000000 ) ) ;
#9352 = CARTESIAN_POINT ( 'NONE',  ( -40.45084971874737789, 39.80000000000000426, -29.38926261462365730 ) ) ;
#9353 = CARTESIAN_POINT ( 'NONE',  ( -50.00000000000000000, 23.78125000068279959, 0.000000000000000000 ) ) ;
#9354 = CARTESIAN_POINT ( 'NONE',  ( -49.86468353124999453, 44.02187500034139589, 16.20201782572377525 ) ) ;
#9355 = CARTESIAN_POINT ( 'NONE',  ( -15.40903463028481646, 25.52187500034139589, -47.42413220539093999 ) ) ;
#9356 = ADVANCED_FACE ( 'NONE', ( #2976 ), #12963, .T. ) ;
#9357 = EDGE_CURVE ( 'NONE', #2833, #8386, #6660, .T. ) ;
#9358 = CARTESIAN_POINT ( 'NONE',  ( -2.547328955960238000E-13, 30.49999999999999645, 49.99999999999999289 ) ) ;
#9359 = ORIENTED_EDGE ( 'NONE', *, *, #10707, .T. ) ;
#9360 = CARTESIAN_POINT ( 'NONE',  ( -49.99999999999999289, 29.68125000068279817, -16.24598481164531449 ) ) ;
#9361 = ORIENTED_EDGE ( 'NONE', *, *, #1633, .F. ) ;
#9362 = EDGE_CURVE ( 'NONE', #9544, #5908, #16074, .T. ) ;
#9363 = PLANE ( 'NONE',  #3652 ) ;
#9364 = LINE ( 'NONE', #11768, #11552 ) ;
#9365 = AXIS2_PLACEMENT_3D ( 'NONE', #14102, #12954, #132 ) ;
#9366 = CARTESIAN_POINT ( 'NONE',  ( -15.45084971874736368, 34.18125000068279462, 47.55282581475768211 ) ) ;
#9367 = CARTESIAN_POINT ( 'NONE',  ( -30.81806926056963292, 47.62187500034139731, -42.41743335407646498 ) ) ;
#9368 = CARTESIAN_POINT ( 'NONE',  ( -30.81806926056962226, 24.15937500034139873, 42.41743335407647919 ) ) ;
#9369 = FACE_OUTER_BOUND ( 'NONE', #15442, .T. ) ;
#9370 = EDGE_CURVE ( 'NONE', #1499, #15672, #7512, .T. ) ;
#9371 = CARTESIAN_POINT ( 'NONE',  ( 40.34137639590981195, 41.12187500034139731, -29.30972558990011834 ) ) ;
#9372 = DIRECTION ( 'NONE',  ( -0.5000000000000039968, -5.069245582283703280E-17, -0.8660254037844363761 ) ) ;
#9373 = CARTESIAN_POINT ( 'NONE',  ( -40.34137639590981195, 46.12187500034139731, 29.30972558990012189 ) ) ;
#9374 = CARTESIAN_POINT ( 'NONE',  ( 0.000000000000000000, 272.0000000000000000, 0.000000000000000000 ) ) ;
#9375 = EDGE_LOOP ( 'NONE', ( #2807, #14128, #11563, #2067 ) ) ;
#9376 = CIRCLE ( 'NONE', #4339, 45.00000000000000000 ) ;
#9377 = CARTESIAN_POINT ( 'NONE',  ( 30.81806926056964002, 40.62187500034139731, 42.41743335407647209 ) ) ;
#9378 = VERTEX_POINT ( 'NONE', #3557 ) ;
#9379 = ORIENTED_EDGE ( 'NONE', *, *, #12255, .T. ) ;
#9380 = ADVANCED_FACE ( 'NONE', ( #3394 ), #11039, .T. ) ;
#9381 = DIRECTION ( 'NONE',  ( 1.000000000000000000, 0.000000000000000000, 0.000000000000000000 ) ) ;
#9382 = LINE ( 'NONE', #4238, #12886 ) ;
#9383 = DIRECTION ( 'NONE',  ( 0.000000000000000000, -1.000000000000000000, 0.000000000000000000 ) ) ;
#9384 = CARTESIAN_POINT ( 'NONE',  ( 15.45084971874737789, 24.60000000000000142, 47.55282581475767500 ) ) ;
#9385 = CARTESIAN_POINT ( 'NONE',  ( -30.81806926056963292, 45.55937500034139731, -42.41743335407647209 ) ) ;
#9386 = CARTESIAN_POINT ( 'NONE',  ( -7.919222016226688865, 31.33250428222963890, -50.00000000000003553 ) ) ;
#9387 = CARTESIAN_POINT ( 'NONE',  ( 0.000000000000000000, 22.50000000000000000, 101.0000000000000000 ) ) ;
#9388 = EDGE_CURVE ( 'NONE', #81, #8272, #14997, .T. ) ;
#9389 = AXIS2_PLACEMENT_3D ( 'NONE', #10145, #2655, #8641 ) ;
#9390 = CARTESIAN_POINT ( 'NONE',  ( 0.000000000000000000, 20.00000000000000355, 50.00000000000000000 ) ) ;
#9391 =( LENGTH_UNIT ( ) NAMED_UNIT ( * ) SI_UNIT ( .MILLI., .METRE. ) );
#9392 = DIRECTION ( 'NONE',  ( 0.000000000000000000, -0.000000000000000000, -1.000000000000000000 ) ) ;
#9393 = CARTESIAN_POINT ( 'NONE',  ( 50.00000000000000711, 34.68125000068279462, 16.24598481164530739 ) ) ;
#9394 = DIRECTION ( 'NONE',  ( 0.000000000000000000, 1.000000000000000000, 0.000000000000000000 ) ) ;
#9395 = CARTESIAN_POINT ( 'NONE',  ( 0.000000000000000000, 32.49999999999998579, -40.00000000000000000 ) ) ;
#9396 = LINE ( 'NONE', #13456, #2988 ) ;
#9397 = VERTEX_POINT ( 'NONE', #10875 ) ;
#9398 = CARTESIAN_POINT ( 'NONE',  ( 40.34137639590981905, 40.65937500034139873, 29.30972558990010768 ) ) ;
#9399 = ORIENTED_EDGE ( 'NONE', *, *, #8684, .T. ) ;
#9400 = ORIENTED_EDGE ( 'NONE', *, *, #7058, .F. ) ;
#9401 = AXIS2_PLACEMENT_3D ( 'NONE', #1130, #3895, #4996 ) ;
#9402 = DIRECTION ( 'NONE',  ( 0.000000000000000000, 1.000000000000000000, 0.000000000000000000 ) ) ;
#9403 = PLANE ( 'NONE',  #13451 ) ;
#9404 = CARTESIAN_POINT ( 'NONE',  ( 49.86468353125001585, 24.75937500034140015, 16.20201782572375038 ) ) ;
#9405 = ORIENTED_EDGE ( 'NONE', *, *, #16062, .T. ) ;
#9406 = CARTESIAN_POINT ( 'NONE',  ( 0.000000000000000000, 20.00000000000000355, 0.000000000000000000 ) ) ;
#9407 = CARTESIAN_POINT ( 'NONE',  ( 30.90169943749475223, 22.69999999999999929, 42.53254041760199300 ) ) ;
#9408 = DIRECTION ( 'NONE',  ( -6.938893903907222461E-16, -1.000000000000000000, 0.000000000000000000 ) ) ;
#9409 = CARTESIAN_POINT ( 'NONE',  ( 15.40903463028481113, 25.32187500034139660, -47.42413220539094709 ) ) ;
#9410 = CARTESIAN_POINT ( 'NONE',  ( -3.111920190527341144E-15, 29.28125000068279604, -50.00000000000000000 ) ) ;
#9411 = CARTESIAN_POINT ( 'NONE',  ( 30.90169943749473802, 47.29999999999999716, -42.53254041760200721 ) ) ;
#9412 = CARTESIAN_POINT ( 'NONE',  ( -48.32661496269150803, 20.00000000000000355, 12.28922088333830054 ) ) ;
#9413 = CARTESIAN_POINT ( 'NONE',  ( -30.81806926056962226, 24.22187500034139518, 42.41743335407647209 ) ) ;
#9414 = DIRECTION ( 'NONE',  ( 1.000000000000000000, 0.000000000000000000, 1.734723475976807094E-17 ) ) ;
#9415 = VECTOR ( 'NONE', #5702, 1000.000000000000000 ) ;
#9416 = CARTESIAN_POINT ( 'NONE',  ( 50.00000000000000000, 37.00000000000000711, -6.123233995736766085E-15 ) ) ;
#9417 = CARTESIAN_POINT ( 'NONE',  ( 15.40903463028482356, 24.45937500034139589, 47.42413220539093999 ) ) ;
#9418 = CARTESIAN_POINT ( 'NONE',  ( 12.83864924538547037, 33.38715533906356114, 101.6666710451724214 ) ) ;
#9419 = VERTEX_POINT ( 'NONE', #12277 ) ;
#9420 = CARTESIAN_POINT ( 'NONE',  ( -15.40903463028480580, 32.25937500034140015, 47.42413220539094709 ) ) ;
#9421 = ORIENTED_EDGE ( 'NONE', *, *, #8226, .T. ) ;
#9422 = DIRECTION ( 'NONE',  ( 0.000000000000000000, 0.000000000000000000, 1.000000000000000000 ) ) ;
#9423 = CARTESIAN_POINT ( 'NONE',  ( 15.40903463028482356, 40.45937500034139589, 47.42413220539093999 ) ) ;
#9424 = AXIS2_PLACEMENT_3D ( 'NONE', #12876, #12546, #7804 ) ;
#9425 = ADVANCED_FACE ( 'NONE', ( #5890 ), #12347, .T. ) ;
#9426 = CARTESIAN_POINT ( 'NONE',  ( 22.46613188259122040, 283.6958662468466059, 8.733065941287961209 ) ) ;
#9427 = DIRECTION ( 'NONE',  ( 1.000000000000000000, 0.000000000000000000, 0.000000000000000000 ) ) ;
#9428 = CARTESIAN_POINT ( 'NONE',  ( 30.81806926056962936, 35.22187500034138452, -42.41743335407647209 ) ) ;
#9429 = CARTESIAN_POINT ( 'NONE',  ( -49.86468353125000164, 35.85937500034140157, 0.000000000000000000 ) ) ;
#9430 = CARTESIAN_POINT ( 'NONE',  ( -30.90169943749474513, 43.70000000000000284, -42.53254041760200721 ) ) ;
#9431 = CARTESIAN_POINT ( 'NONE',  ( 30.81806926056964002, 32.62187500034140442, 42.41743335407647209 ) ) ;
#9432 = CARTESIAN_POINT ( 'NONE',  ( -50.00000000000000000, 44.00000000000000711, 0.000000000000000000 ) ) ;
#9433 = CARTESIAN_POINT ( 'NONE',  ( -30.90169943749474868, 21.48125000068279533, -42.53254041760200721 ) ) ;
#9434 = CARTESIAN_POINT ( 'NONE',  ( 49.86468353124999453, 45.02187500034138878, -16.20201782572376459 ) ) ;
#9435 = AXIS2_PLACEMENT_3D ( 'NONE', #9292, #8031, #5564 ) ;
#9436 = AXIS2_PLACEMENT_3D ( 'NONE', #8802, #11541, #9056 ) ;
#9437 = CARTESIAN_POINT ( 'NONE',  ( 40.34137639590981195, 23.12187500034139731, -29.30972558990011834 ) ) ;
#9438 = ADVANCED_FACE ( 'NONE', ( #9798 ), #7303, .F. ) ;
#9439 = CARTESIAN_POINT ( 'NONE',  ( 40.34137639590981195, 49.05937500034139731, -29.30972558990011834 ) ) ;
#9440 = VERTEX_POINT ( 'NONE', #3476 ) ;
#9441 = CARTESIAN_POINT ( 'NONE',  ( 15.45084971874737789, 30.38125000068280102, 47.55282581475767500 ) ) ;
#9442 = ORIENTED_EDGE ( 'NONE', *, *, #14467, .T. ) ;
#9443 = CARTESIAN_POINT ( 'NONE',  ( 0.000000000000000000, 52.00000000000000711, -50.00000000000000000 ) ) ;
#9444 = AXIS2_PLACEMENT_3D ( 'NONE', #3691, #925, #7352 ) ;
#9445 = CARTESIAN_POINT ( 'NONE',  ( 49.86468353125001585, 38.82187500034140015, 16.20201782572375038 ) ) ;
#9446 = CARTESIAN_POINT ( 'NONE',  ( -30.81806926056963292, 23.55937500034139376, -42.41743335407647209 ) ) ;
#9447 = EDGE_CURVE ( 'NONE', #14378, #14510, #3302, .T. ) ;
#9448 = PRESENTATION_LAYER_ASSIGNMENT (  '', '', ( #12359 ) ) ;
#9449 = CARTESIAN_POINT ( 'NONE',  ( -49.99999999999999289, 39.88125000068280457, 16.24598481164533226 ) ) ;
#9450 = CONTEXT_DEPENDENT_SHAPE_REPRESENTATION ( #14912, #15685 ) ;
#9451 = CARTESIAN_POINT ( 'NONE',  ( -50.00000000000000000, 40.00000000000000000, 0.000000000000000000 ) ) ;
#9452 = CARTESIAN_POINT ( 'NONE',  ( 15.40903463028482356, 46.52187500034139589, 47.42413220539093999 ) ) ;
#9453 = CARTESIAN_POINT ( 'NONE',  ( -50.00000000000000000, 45.78125000068279604, 0.000000000000000000 ) ) ;
#9454 = VECTOR ( 'NONE', #14849, 1000.000000000000000 ) ;
#9455 = CIRCLE ( 'NONE', #11581, 45.00000000000000000 ) ;
#9456 = ORIENTED_EDGE ( 'NONE', *, *, #8434, .T. ) ;
#9457 = AXIS2_PLACEMENT_3D ( 'NONE', #9703, #11032, #796 ) ;
#9458 = CARTESIAN_POINT ( 'NONE',  ( 40.34137639590981905, 40.72187500034139873, 29.30972558990010768 ) ) ;
#9459 = PRODUCT_DEFINITION_SHAPE ( 'NONE', 'NONE',  #16473 ) ;
#9460 = EDGE_LOOP ( 'NONE', ( #10872, #11270, #1162, #12342 ) ) ;
#9461 = ORIENTED_EDGE ( 'NONE', *, *, #13222, .T. ) ;
#9462 = EDGE_CURVE ( 'NONE', #3391, #1181, #4822, .T. ) ;
#9463 = LINE ( 'NONE', #8212, #2850 ) ;
#9464 = LINE ( 'NONE', #231, #15537 ) ;
#9465 = DIRECTION ( 'NONE',  ( 0.000000000000000000, 0.000000000000000000, 1.000000000000000000 ) ) ;
#9466 = DIRECTION ( 'NONE',  ( 0.3420201433256698231, 0.6644630243886754384, -0.6644630243886734400 ) ) ;
#9467 = AXIS2_PLACEMENT_3D ( 'NONE', #260, #15562, #6861 ) ;
#9468 = CARTESIAN_POINT ( 'NONE',  ( 49.86468353124999453, 46.95937500034139589, -16.20201782572376459 ) ) ;
#9469 = AXIS2_PLACEMENT_3D ( 'NONE', #13911, #14247, #9427 ) ;
#9470 = AXIS2_PLACEMENT_3D ( 'NONE', #1148, #2729, #7807 ) ;
#9471 = CARTESIAN_POINT ( 'NONE',  ( -15.40903463028481646, 47.45937500034139589, -47.42413220539093999 ) ) ;
#9472 = LINE ( 'NONE', #8140, #9272 ) ;
#9473 = AXIS2_PLACEMENT_3D ( 'NONE', #6678, #4337, #13138 ) ;
#9474 = CARTESIAN_POINT ( 'NONE',  ( -7.919222016226822092, 46.44874571845315359, 50.00000000000000000 ) ) ;
#9475 =( NAMED_UNIT ( * ) SI_UNIT ( $, .STERADIAN. ) SOLID_ANGLE_UNIT ( ) );
#9476 = DIRECTION ( 'NONE',  ( 0.1045284632676570929, -0.9945218953682730678, 0.000000000000000000 ) ) ;
#9477 = SHAPE_REPRESENTATION ( 'container base & motor', ( #15812 ), #1480 ) ;
#9478 = FACE_OUTER_BOUND ( 'NONE', #11128, .T. ) ;
#9479 = EDGE_CURVE ( 'NONE', #2769, #5002, #12199, .T. ) ;
#9480 = CARTESIAN_POINT ( 'NONE',  ( 7.919222016226940219, 21.22999571913595673, -49.99999999999996447 ) ) ;
#9481 = DIRECTION ( 'NONE',  ( 0.000000000000000000, 0.000000000000000000, -1.000000000000000000 ) ) ;
#9482 = EDGE_LOOP ( 'NONE', ( #5334, #15303 ) ) ;
#9483 = CARTESIAN_POINT ( 'NONE',  ( -49.86468353124999453, 29.95937500034139944, 16.20201782572377525 ) ) ;
#9484 = AXIS2_PLACEMENT_3D ( 'NONE', #5346, #3065, #12973 ) ;
#9485 = VECTOR ( 'NONE', #16407, 1000.000000000000000 ) ;
#9486 = ORIENTED_EDGE ( 'NONE', *, *, #1120, .F. ) ;
#9487 = EDGE_LOOP ( 'NONE', ( #10083, #2954 ) ) ;
#9488 = ORIENTED_EDGE ( 'NONE', *, *, #15187, .T. ) ;
#9489 = CIRCLE ( 'NONE', #4993, 89.78914894885470233 ) ;
#9490 = CARTESIAN_POINT ( 'NONE',  ( -40.45084971874737079, 47.98125000068279888, 29.38926261462367151 ) ) ;
#9491 = LINE ( 'NONE', #7905, #8155 ) ;
#9492 = LINE ( 'NONE', #1825, #7304 ) ;
#9493 = ORIENTED_EDGE ( 'NONE', *, *, #1358, .T. ) ;
#9494 = LINE ( 'NONE', #11898, #8656 ) ;
#9495 = DIRECTION ( 'NONE',  ( -0.000000000000000000, -1.000000000000000000, -0.000000000000000000 ) ) ;
#9496 = FACE_OUTER_BOUND ( 'NONE', #2994, .T. ) ;
#9497 = CARTESIAN_POINT ( 'NONE',  ( -40.34137639590981905, 27.72187500034139873, -29.30972558990011478 ) ) ;
#9498 = CARTESIAN_POINT ( 'NONE',  ( 40.45084971874737789, 38.80000000000000426, 29.38926261462365375 ) ) ;
#9499 = CARTESIAN_POINT ( 'NONE',  ( 17.27465264870989259, 19.64379522392349031, 94.97817908659912689 ) ) ;
#9500 = CARTESIAN_POINT ( 'NONE',  ( -47.93512317712408333, 19.99999999999999645, 13.73719875613861241 ) ) ;
#9501 = EDGE_CURVE ( 'NONE', #6818, #1658, #879, .T. ) ;
#9502 = CARTESIAN_POINT ( 'NONE',  ( 40.34137639590981195, 23.12187500034139731, -29.30972558990011834 ) ) ;
#9503 = DIRECTION ( 'NONE',  ( 0.9510565162951503115, 0.3090169943749573878, 0.000000000000000000 ) ) ;
#9504 = EDGE_CURVE ( 'NONE', #12958, #12158, #10492, .T. ) ;
#9505 = CARTESIAN_POINT ( 'NONE',  ( 15.45084971874736723, 33.39999999999999858, -47.55282581475768211 ) ) ;
#9506 = CARTESIAN_POINT ( 'NONE',  ( -40.34137639590981195, 24.05937500034139731, 29.30972558990012189 ) ) ;
#9507 = CARTESIAN_POINT ( 'NONE',  ( -49.86468353124999453, 49.75937500034138594, -16.20201782572375393 ) ) ;
#9508 = VERTEX_POINT ( 'NONE', #2128 ) ;
#9509 = CARTESIAN_POINT ( 'NONE',  ( -30.81806926056962226, 32.15937500034139873, 42.41743335407647209 ) ) ;
#9510 = ORIENTED_EDGE ( 'NONE', *, *, #11413, .F. ) ;
#9511 = CARTESIAN_POINT ( 'NONE',  ( -43.87482193696060762, 257.0000000000001137, 10.00000000000000178 ) ) ;
#9512 = CARTESIAN_POINT ( 'NONE',  ( 49.86468353124999453, 38.95937500034139589, -16.20201782572376459 ) ) ;
#9513 = CARTESIAN_POINT ( 'NONE',  ( 28.69101924422353989, 282.0322304394514958, 11.84550962211153724 ) ) ;
#9514 = EDGE_CURVE ( 'NONE', #10158, #2051, #12115, .T. ) ;
#9515 = CARTESIAN_POINT ( 'NONE',  ( -23.90010208165381655, 283.0244618719127629, 9.450051040827698756 ) ) ;
#9516 = ADVANCED_FACE ( 'NONE', ( #14927 ), #9711, .F. ) ;
#9517 = CARTESIAN_POINT ( 'NONE',  ( 15.40903463028481113, 27.32187500034139660, -47.42413220539094709 ) ) ;
#9518 = CARTESIAN_POINT ( 'NONE',  ( 9.631387414534489405E-15, 38.35937500034139447, 52.43083105670540789 ) ) ;
#9519 = CARTESIAN_POINT ( 'NONE',  ( -40.45084971874737079, 44.20000000000000284, 29.38926261462367151 ) ) ;
#9520 = CARTESIAN_POINT ( 'NONE',  ( -30.81806926056962226, 32.22187500034139163, 42.41743335407647919 ) ) ;
#9521 = CARTESIAN_POINT ( 'NONE',  ( 9.657523855033129090E-15, 42.50000000000000711, 52.57311121191334990 ) ) ;
#9522 = CARTESIAN_POINT ( 'NONE',  ( -30.81806926056963292, 45.55937500034139731, -42.41743335407647209 ) ) ;
#9523 = CARTESIAN_POINT ( 'NONE',  ( -49.86468353124999453, 42.02187500034139589, 16.20201782572377525 ) ) ;
#9524 = ADVANCED_FACE ( 'NONE', ( #5973 ), #8608, .T. ) ;
#9525 = CARTESIAN_POINT ( 'NONE',  ( -49.86468353124999453, 21.82187500034139305, -16.20201782572375393 ) ) ;
#9526 = VERTEX_POINT ( 'NONE', #12028 ) ;
#9527 = CARTESIAN_POINT ( 'NONE',  ( -15.40903463028481646, 49.45937500034140299, -47.42413220539093999 ) ) ;
#9528 = ORIENTED_EDGE ( 'NONE', *, *, #10122, .T. ) ;
#9529 = ORIENTED_EDGE ( 'NONE', *, *, #6958, .F. ) ;
#9530 = CARTESIAN_POINT ( 'NONE',  ( 30.90169943749474157, 31.08125000068280031, -42.53254041760200721 ) ) ;
#9531 = VECTOR ( 'NONE', #11451, 1000.000000000000000 ) ;
#9532 = ORIENTED_EDGE ( 'NONE', *, *, #534, .F. ) ;
#9533 = CARTESIAN_POINT ( 'NONE',  ( 6.123233995736766085E-15, 20.00000000000000355, -50.00000000000000000 ) ) ;
#9534 = CARTESIAN_POINT ( 'NONE',  ( 30.90169943749473802, 33.08125000068279320, -42.53254041760200721 ) ) ;
#9535 = CARTESIAN_POINT ( 'NONE',  ( 15.40903463028482356, 42.52187500034139589, 47.42413220539093999 ) ) ;
#9536 = CARTESIAN_POINT ( 'NONE',  ( 49.86468353124999453, 47.02187500034139589, -16.20201782572376459 ) ) ;
#9537 = CARTESIAN_POINT ( 'NONE',  ( -1.790468199911974034, 98.25246584726781407, -9.080892972013931086 ) ) ;
#9538 = CARTESIAN_POINT ( 'NONE',  ( -49.99999999999999289, 37.90000000000000568, -16.24598481164531449 ) ) ;
#9539 = TOROIDAL_SURFACE ( 'NONE', #11139, 88.87749532708107836, 2.000000000000000000 ) ;
#9540 = CARTESIAN_POINT ( 'NONE',  ( -49.86468353124999453, 39.82187500034140015, -16.20201782572375393 ) ) ;
#9541 = FACE_OUTER_BOUND ( 'NONE', #7514, .T. ) ;
#9542 = EDGE_LOOP ( 'NONE', ( #4541, #12694 ) ) ;
#9543 = CARTESIAN_POINT ( 'NONE',  ( -15.40903463028481646, 43.52187500034139589, -47.42413220539093999 ) ) ;
#9544 = VERTEX_POINT ( 'NONE', #628 ) ;
#9545 = VERTEX_POINT ( 'NONE', #5725 ) ;
#9546 = ORIENTED_EDGE ( 'NONE', *, *, #3052, .F. ) ;
#9547 = CARTESIAN_POINT ( 'NONE',  ( 0.000000000000000000, 20.00000000000000355, -40.00000000000000000 ) ) ;
#9548 = LINE ( 'NONE', #3219, #13156 ) ;
#9549 = CARTESIAN_POINT ( 'NONE',  ( 0.000000000000000000, 52.00000000000000711, 0.000000000000000000 ) ) ;
#9550 = CARTESIAN_POINT ( 'NONE',  ( -8.487905985326078095, 95.47132599478250370, -3.471325994782476609 ) ) ;
#9551 = CIRCLE ( 'NONE', #4518, 49.99999999999999289 ) ;
#9552 = CARTESIAN_POINT ( 'NONE',  ( 9.631387414534489405E-15, 44.35937500034140157, 52.43083105670540789 ) ) ;
#9553 = CARTESIAN_POINT ( 'NONE',  ( 30.81806926056964002, 46.55937500034139020, 42.41743335407646498 ) ) ;
#9554 = CARTESIAN_POINT ( 'NONE',  ( -30.90169943749474513, 29.69999999999999929, -42.53254041760200721 ) ) ;
#9555 = CARTESIAN_POINT ( 'NONE',  ( -15.45084971874737256, 33.38125000068280457, -47.55282581475767500 ) ) ;
#9556 = PRESENTATION_STYLE_ASSIGNMENT (( #8221 ) ) ;
#9557 = CARTESIAN_POINT ( 'NONE',  ( 2.500000000000000000, 242.0000000000000284, -47.99999999999999289 ) ) ;
#9558 = CARTESIAN_POINT ( 'NONE',  ( 0.000000000000000000, 20.00000000000000355, 0.000000000000000000 ) ) ;
#9559 = EDGE_CURVE ( 'NONE', #8721, #14669, #9548, .T. ) ;
#9560 = CARTESIAN_POINT ( 'NONE',  ( -15.45084971874736368, 34.39999999999999858, 47.55282581475768211 ) ) ;
#9561 = DIRECTION ( 'NONE',  ( 0.000000000000000000, 1.000000000000000000, 0.000000000000000000 ) ) ;
#9562 = EDGE_LOOP ( 'NONE', ( #15113, #14030, #9640 ) ) ;
#9563 = CARTESIAN_POINT ( 'NONE',  ( 9.631387414534489405E-15, 30.35937500034139447, 52.43083105670540789 ) ) ;
#9564 = ORIENTED_EDGE ( 'NONE', *, *, #6034, .F. ) ;
#9565 = ORIENTED_EDGE ( 'NONE', *, *, #2391, .F. ) ;
#9566 = EDGE_LOOP ( 'NONE', ( #12197, #13679, #9812 ) ) ;
#9567 = EDGE_CURVE ( 'NONE', #6897, #11171, #6002, .T. ) ;
#9568 = EDGE_CURVE ( 'NONE', #11934, #13988, #8368, .T. ) ;
#9569 = CARTESIAN_POINT ( 'NONE',  ( -3.219174618344376363E-15, 43.28125000068280315, -52.57311121191334990 ) ) ;
#9570 = CARTESIAN_POINT ( 'NONE',  ( 9.574901606694759531E-15, 52.00000000000001421, -2.191293403013901163E-14 ) ) ;
#9571 = DIRECTION ( 'NONE',  ( -0.000000000000000000, -1.000000000000000000, -0.000000000000000000 ) ) ;
#9572 = ORIENTED_EDGE ( 'NONE', *, *, #5864, .T. ) ;
#9573 = EDGE_CURVE ( 'NONE', #5931, #8153, #5147, .T. ) ;
#9574 = FACE_OUTER_BOUND ( 'NONE', #5767, .T. ) ;
#9575 = LINE ( 'NONE', #14619, #11562 ) ;
#9576 = CARTESIAN_POINT ( 'NONE',  ( 0.000000000000000000, 20.00000000000000355, 0.000000000000000000 ) ) ;
#9577 = DIRECTION ( 'NONE',  ( 0.000000000000000000, 0.000000000000000000, -1.000000000000000000 ) ) ;
#9578 = CARTESIAN_POINT ( 'NONE',  ( 6.123233995736766085E-15, 193.4213562373095385, 50.00000000000000000 ) ) ;
#9579 = DIRECTION ( 'NONE',  ( -0.8660254037844327124, 0.000000000000000000, 0.5000000000000102141 ) ) ;
#9580 = LINE ( 'NONE', #909, #5687 ) ;
#9581 = CARTESIAN_POINT ( 'NONE',  ( 49.86468353125001585, 20.82187500034140015, 16.20201782572375038 ) ) ;
#9582 = CARTESIAN_POINT ( 'NONE',  ( 2.518620260143848100, 35.01862026014384099, 40.00000000000000711 ) ) ;
#9583 = ADVANCED_FACE ( 'NONE', ( #1209 ), #4985, .T. ) ;
#9584 = CARTESIAN_POINT ( 'NONE',  ( 49.99999999999999289, 33.10000000000000853, -16.24598481164532160 ) ) ;
#9585 = CARTESIAN_POINT ( 'NONE',  ( 15.40903463028481113, 23.25937500034139660, -47.42413220539094709 ) ) ;
#9586 = CARTESIAN_POINT ( 'NONE',  ( -3.111920190527341144E-15, 29.50000000000000000, -50.00000000000000000 ) ) ;
#9587 = ORIENTED_EDGE ( 'NONE', *, *, #15336, .F. ) ;
#9588 = LINE ( 'NONE', #15901, #14192 ) ;
#9589 = EDGE_LOOP ( 'NONE', ( #11949, #16282, #1310, #778 ) ) ;
#9590 = CARTESIAN_POINT ( 'NONE',  ( 0.000000000000000000, 247.0000000000000284, 45.00000000000000000 ) ) ;
#9591 = CARTESIAN_POINT ( 'NONE',  ( -40.34137639590981195, 44.05937500034139731, 29.30972558990012189 ) ) ;
#9592 = CARTESIAN_POINT ( 'NONE',  ( 15.45084971874737789, 28.38125000068279746, 47.55282581475767500 ) ) ;
#9593 = CARTESIAN_POINT ( 'NONE',  ( 0.000000000000000000, 245.0000000000000284, 47.99999999999999289 ) ) ;
#9594 = CARTESIAN_POINT ( 'NONE',  ( 9.631387414534489405E-15, 26.42187500034139447, 52.43083105670540789 ) ) ;
#9595 = CARTESIAN_POINT ( 'NONE',  ( 40.34137639590981195, 33.05937500034139731, -29.30972558990011834 ) ) ;
#9596 = FACE_OUTER_BOUND ( 'NONE', #8762, .T. ) ;
#9597 = CARTESIAN_POINT ( 'NONE',  ( -15.40903463028481646, 33.52187500034140299, -47.42413220539093999 ) ) ;
#9598 = FACE_OUTER_BOUND ( 'NONE', #15252, .T. ) ;
#9599 = CARTESIAN_POINT ( 'NONE',  ( -30.81806926056962226, 42.15937500034139163, 42.41743335407647919 ) ) ;
#9600 = CARTESIAN_POINT ( 'NONE',  ( 40.34137639590981195, 39.12187500034139731, -29.30972558990011834 ) ) ;
#9601 = CARTESIAN_POINT ( 'NONE',  ( -3.210462471511496205E-15, 21.42187500034139802, -52.43083105670540789 ) ) ;
#9602 = VERTEX_POINT ( 'NONE', #12696 ) ;
#9603 = CARTESIAN_POINT ( 'NONE',  ( 49.86468353125000164, 48.85937500034139447, -6.106662507704105588E-15 ) ) ;
#9604 = ORIENTED_EDGE ( 'NONE', *, *, #11870, .T. ) ;
#9605 = EDGE_LOOP ( 'NONE', ( #3781, #10994 ) ) ;
#9606 = CARTESIAN_POINT ( 'NONE',  ( -50.00000000000000000, 33.78125000068280315, 0.000000000000000000 ) ) ;
#9607 = ORIENTED_EDGE ( 'NONE', *, *, #4378, .F. ) ;
#9608 = CYLINDRICAL_SURFACE ( 'NONE', #15006, 50.00000000000000000 ) ;
#9609 = CARTESIAN_POINT ( 'NONE',  ( -49.86468353125000164, 39.92187500034139447, 0.000000000000000000 ) ) ;
#9610 = ADVANCED_FACE ( 'NONE', ( #43 ), #8955, .F. ) ;
#9611 = CARTESIAN_POINT ( 'NONE',  ( -49.86468353124999453, 49.82187500034140015, -16.20201782572375393 ) ) ;
#9612 = DIRECTION ( 'NONE',  ( 0.000000000000000000, 0.000000000000000000, 1.000000000000000000 ) ) ;
#9613 = CARTESIAN_POINT ( 'NONE',  ( -30.81806926056963292, 25.62187500034139731, -42.41743335407647209 ) ) ;
#9614 = CARTESIAN_POINT ( 'NONE',  ( -49.99999999999999289, 40.09999999999999432, 16.24598481164533226 ) ) ;
#9615 = CARTESIAN_POINT ( 'NONE',  ( -30.81806926056963292, 41.62187500034139020, -42.41743335407647209 ) ) ;
#9616 = DIRECTION ( 'NONE',  ( -1.000000000000000000, 0.000000000000000000, 1.156482317317871478E-16 ) ) ;
#9617 = EDGE_LOOP ( 'NONE', ( #4557, #1561, #8475, #15544 ) ) ;
#9618 = CARTESIAN_POINT ( 'NONE',  ( -40.34137639590981905, 39.72187500034139873, -29.30972558990011478 ) ) ;
#9619 = ORIENTED_EDGE ( 'NONE', *, *, #15346, .T. ) ;
#9620 = VERTEX_POINT ( 'NONE', #1294 ) ;
#9621 = ORIENTED_EDGE ( 'NONE', *, *, #1214, .F. ) ;
#9622 = FACE_OUTER_BOUND ( 'NONE', #2999, .T. ) ;
#9623 = CARTESIAN_POINT ( 'NONE',  ( 15.84787772126904137, 28.17501872725030054, 101.6666710451724214 ) ) ;
#9624 = CARTESIAN_POINT ( 'NONE',  ( -50.00000000000000000, 49.78125000068280315, 0.000000000000000000 ) ) ;
#9625 = CARTESIAN_POINT ( 'NONE',  ( -2.168404344971008868E-16, 282.0000000000000000, -12.50000000000000000 ) ) ;
#9626 = CARTESIAN_POINT ( 'NONE',  ( -49.86468353124999453, 35.95937500034139589, 16.20201782572377525 ) ) ;
#9627 = CARTESIAN_POINT ( 'NONE',  ( -49.86468353125000164, 45.85937500034140157, 0.000000000000000000 ) ) ;
#9628 = DIRECTION ( 'NONE',  ( 1.000000000000000000, 0.000000000000000000, 0.000000000000000000 ) ) ;
#9629 = DIRECTION ( 'NONE',  ( 0.000000000000000000, 1.000000000000000000, 0.000000000000000000 ) ) ;
#9630 = DIRECTION ( 'NONE',  ( 0.4067366430758010964, -0.9135454576426004225, 0.000000000000000000 ) ) ;
#9631 = CARTESIAN_POINT ( 'NONE',  ( 0.000000000000000000, 50.00000000000000000, 0.000000000000000000 ) ) ;
#9632 = CARTESIAN_POINT ( 'NONE',  ( 50.00000000000000711, 36.89999999999999858, 16.24598481164530739 ) ) ;
#9633 = FACE_OUTER_BOUND ( 'NONE', #5906, .T. ) ;
#9634 = VERTEX_POINT ( 'NONE', #13683 ) ;
#9635 = ADVANCED_FACE ( 'NONE', ( #2380 ), #16266, .T. ) ;
#9636 = CARTESIAN_POINT ( 'NONE',  ( -3.210462471511496205E-15, 33.35937500034140157, -52.43083105670540789 ) ) ;
#9637 = EDGE_CURVE ( 'NONE', #10236, #1407, #11287, .T. ) ;
#9638 = VERTEX_POINT ( 'NONE', #10044 ) ;
#9639 = VERTEX_POINT ( 'NONE', #12529 ) ;
#9640 = ORIENTED_EDGE ( 'NONE', *, *, #5400, .F. ) ;
#9641 = CARTESIAN_POINT ( 'NONE',  ( -15.45084971874736368, 42.18125000068279462, 47.55282581475768211 ) ) ;
#9642 = CARTESIAN_POINT ( 'NONE',  ( -30.90169943749474513, 39.69999999999999574, -42.53254041760200721 ) ) ;
#9643 = FACE_OUTER_BOUND ( 'NONE', #7120, .T. ) ;
#9644 = VERTEX_POINT ( 'NONE', #1375 ) ;
#9645 = CARTESIAN_POINT ( 'NONE',  ( -15.45084971874736368, 38.40000000000000568, 47.55282581475768211 ) ) ;
#9646 = LINE ( 'NONE', #8481, #11165 ) ;
#9647 = LINE ( 'NONE', #14699, #11835 ) ;
#9648 = LINE ( 'NONE', #13626, #6536 ) ;
#9649 = CYLINDRICAL_SURFACE ( 'NONE', #4082, 47.00000000000000000 ) ;
#9650 = CARTESIAN_POINT ( 'NONE',  ( 16.79799753235259985, 27.43226914341417810, 102.0000000000000142 ) ) ;
#9651 = CARTESIAN_POINT ( 'NONE',  ( 15.45084971874737789, 38.60000000000000142, 47.55282581475767500 ) ) ;
#9652 = CARTESIAN_POINT ( 'NONE',  ( 30.90169943749473802, 37.08125000068280031, -42.53254041760200721 ) ) ;
#9653 = EDGE_CURVE ( 'NONE', #7385, #8473, #10456, .T. ) ;
#9654 = DIRECTION ( 'NONE',  ( -0.000000000000000000, -1.000000000000000000, -0.000000000000000000 ) ) ;
#9655 = CARTESIAN_POINT ( 'NONE',  ( 49.86468353124999453, 25.02187500034139589, -16.20201782572376104 ) ) ;
#9656 = DIRECTION ( 'NONE',  ( -0.000000000000000000, -1.000000000000000000, -0.000000000000000000 ) ) ;
#9657 = CARTESIAN_POINT ( 'NONE',  ( 40.45084971874737079, 31.20000000000000284, -29.38926261462366440 ) ) ;
#9658 = CARTESIAN_POINT ( 'NONE',  ( -49.86468353124999453, 25.75937500034140015, -16.20201782572375393 ) ) ;
#9659 = AXIS2_PLACEMENT_3D ( 'NONE', #6771, #5526, #11981 ) ;
#9660 = CARTESIAN_POINT ( 'NONE',  ( 9.574901606694759531E-15, 52.00000000000001421, 34.99999999999999289 ) ) ;
#9661 = EDGE_LOOP ( 'NONE', ( #2294, #1472, #6995, #4501 ) ) ;
#9662 = CARTESIAN_POINT ( 'NONE',  ( 9.631387414534489405E-15, 26.35937500034139802, 52.43083105670540789 ) ) ;
#9663 = ORIENTED_EDGE ( 'NONE', *, *, #8150, .T. ) ;
#9664 = DIRECTION ( 'NONE',  ( 0.000000000000000000, 1.000000000000000000, 0.000000000000000000 ) ) ;
#9666 =( BOUNDED_CURVE ( )  B_SPLINE_CURVE ( 2, ( #6530, #16248, #4882, #27, #6200, #16330, #2442, #1187, #6285, #10107, #11356, #16421, #15159 ),
 .UNSPECIFIED., .F., .F. ) 
 B_SPLINE_CURVE_WITH_KNOTS ( ( 3, 2, 2, 2, 2, 2, 3 ),
 ( 0.5166666666666667185, 0.5200000000000000178, 0.5266666666666666163, 0.5333333333333333259, 0.5400000000000000355, 0.5466666666666666341, 0.5500000000000000444 ),
 .UNSPECIFIED. ) 
 CURVE ( )  GEOMETRIC_REPRESENTATION_ITEM ( )  RATIONAL_B_SPLINE_CURVE ( ( 0.9755282581475768211, 0.9755282581475771542, 1.000000000000000000, 0.9510565162951535312, 1.000000000000000000, 0.9510565162951535312, 1.000000000000000000, 0.9510565162951535312, 1.000000000000000000, 0.9510565162951535312, 1.000000000000000000, 0.9755282581475763770, 0.9755282581475768211 ) ) 
 REPRESENTATION_ITEM ( '' )  );
#9665 = CARTESIAN_POINT ( 'NONE',  ( -30.81806926056962226, 38.15937500034138452, 42.41743335407647919 ) ) ;
#9667 = EDGE_CURVE ( 'NONE', #11385, #5080, #16018, .T. ) ;
#9668 = DIRECTION ( 'NONE',  ( -0.000000000000000000, -1.000000000000000000, -0.000000000000000000 ) ) ;
#9669 = DIRECTION ( 'NONE',  ( 0.000000000000000000, -1.000000000000000000, 0.000000000000000000 ) ) ;
#9670 = VECTOR ( 'NONE', #9721, 1000.000000000000000 ) ;
#9671 = CARTESIAN_POINT ( 'NONE',  ( 0.000000000000000000, 52.00000000000000711, 0.000000000000000000 ) ) ;
#9672 = CARTESIAN_POINT ( 'NONE',  ( -49.86468353124999453, 30.02187500034139234, 16.20201782572377525 ) ) ;
#9673 = CARTESIAN_POINT ( 'NONE',  ( 49.86468353124999453, 30.95937500034139944, -16.20201782572376104 ) ) ;
#9674 = CARTESIAN_POINT ( 'NONE',  ( 0.000000000000000000, 20.00000000000000355, 50.00000000000000000 ) ) ;
#9675 = CARTESIAN_POINT ( 'NONE',  ( 15.40903463028482356, 28.52187500034139589, 47.42413220539093999 ) ) ;
#9676 = CARTESIAN_POINT ( 'NONE',  ( -22.37674264578617311, 24.85189042352198285, 101.0000000000000000 ) ) ;
#9677 = EDGE_CURVE ( 'NONE', #13617, #3799, #3963, .T. ) ;
#9678 = CARTESIAN_POINT ( 'NONE',  ( 9.631387414534489405E-15, 44.35937500034140157, 52.43083105670540789 ) ) ;
#9679 = CARTESIAN_POINT ( 'NONE',  ( 49.86468353125001585, 34.82187500034140015, 16.20201782572375038 ) ) ;
#9680 = EDGE_CURVE ( 'NONE', #3901, #8154, #2546, .T. ) ;
#9681 = CARTESIAN_POINT ( 'NONE',  ( -49.86468353124999453, 20.02187500034139589, 16.20201782572377525 ) ) ;
#9682 = VERTEX_POINT ( 'NONE', #10203 ) ;
#9683 = AXIS2_PLACEMENT_3D ( 'NONE', #12863, #10298, #11530 ) ;
#9684 = CARTESIAN_POINT ( 'NONE',  ( 9.631387414534489405E-15, 40.35937500034139447, 52.43083105670540789 ) ) ;
#9685 = VERTEX_POINT ( 'NONE', #7388 ) ;
#9686 = CARTESIAN_POINT ( 'NONE',  ( 15.45084971874736723, 27.18125000068279817, -47.55282581475768211 ) ) ;
#9687 = ORIENTED_EDGE ( 'NONE', *, *, #1165, .T. ) ;
#9688 = CARTESIAN_POINT ( 'NONE',  ( -49.99999999999999289, 36.10000000000000142, 16.24598481164533226 ) ) ;
#9689 = CARTESIAN_POINT ( 'NONE',  ( 30.81806926056964002, 42.62187500034139731, 42.41743335407646498 ) ) ;
#9690 = CARTESIAN_POINT ( 'NONE',  ( 30.81806926056962936, 49.22187500034139873, -42.41743335407647209 ) ) ;
#9691 = AXIS2_PLACEMENT_3D ( 'NONE', #10698, #5794, #462 ) ;
#9692 = DIRECTION ( 'NONE',  ( -0.000000000000000000, 1.000000000000000000, -0.000000000000000000 ) ) ;
#9693 = AXIS2_PLACEMENT_3D ( 'NONE', #9245, #15632, #10577 ) ;
#9694 = CARTESIAN_POINT ( 'NONE',  ( -49.86468353124999453, 21.82187500034139305, -16.20201782572375393 ) ) ;
#9695 = ITEM_DEFINED_TRANSFORMATION ( 'NONE', 'NONE', #3630,  #15812 ) ;
#9696 = CARTESIAN_POINT ( 'NONE',  ( -15.45084971874737256, 33.38125000068280457, -47.55282581475767500 ) ) ;
#9697 = CARTESIAN_POINT ( 'NONE',  ( -30.90169943749473802, 38.29999999999999716, 42.53254041760200721 ) ) ;
#9698 = EDGE_CURVE ( 'NONE', #13963, #4275, #1044, .T. ) ;
#9699 = CARTESIAN_POINT ( 'NONE',  ( 30.81806926056962936, 43.22187500034140584, -42.41743335407647209 ) ) ;
#9700 = CARTESIAN_POINT ( 'NONE',  ( 6.123233995736766085E-15, 50.00000000000000000, 50.00000000000000000 ) ) ;
#9701 = ORIENTED_EDGE ( 'NONE', *, *, #6628, .F. ) ;
#9702 = CARTESIAN_POINT ( 'NONE',  ( 30.81806926056964002, 44.62187500034140442, 42.41743335407647209 ) ) ;
#9703 = CARTESIAN_POINT ( 'NONE',  ( 8.660254037844387298, 28.00000000000000355, 5.000000000000000000 ) ) ;
#9704 = VERTEX_POINT ( 'NONE', #4898 ) ;
#9705 = ORIENTED_EDGE ( 'NONE', *, *, #13316, .F. ) ;
#9706 = AXIS2_PLACEMENT_3D ( 'NONE', #12346, #8689, #13427 ) ;
#9707 = CIRCLE ( 'NONE', #398, 16.50000000000000711 ) ;
#9708 = ORIENTED_EDGE ( 'NONE', *, *, #12429, .T. ) ;
#9709 = COLOUR_RGB ( '', 0.08235294, 0.09019608, 0.10196078) ;
#9710 = LINE ( 'NONE', #7052, #13722 ) ;
#9711 = PLANE ( 'NONE',  #656 ) ;
#9712 = CARTESIAN_POINT ( 'NONE',  ( -40.45084971874737079, 21.98125000068279888, 29.38926261462367151 ) ) ;
#9713 = FACE_OUTER_BOUND ( 'NONE', #14688, .T. ) ;
#9714 = CARTESIAN_POINT ( 'NONE',  ( -49.86468353124999453, 37.95937500034140299, 16.20201782572377525 ) ) ;
#9715 = CARTESIAN_POINT ( 'NONE',  ( 40.34137639590981195, 49.05937500034139731, -29.30972558990011834 ) ) ;
#9716 = DIRECTION ( 'NONE',  ( -0.9135454576426004225, -0.4067366430758009854, 0.000000000000000000 ) ) ;
#9717 = DIRECTION ( 'NONE',  ( -1.000000000000000000, 0.000000000000000000, 0.000000000000000000 ) ) ;
#9718 = SHAPE_REPRESENTATION_RELATIONSHIP ( 'NONE' , 'NONE' ,  #13496, #1259 ) ;
#9719 = CIRCLE ( 'NONE', #12636, 82.49773270518484480 ) ;
#9721 = DIRECTION ( 'NONE',  ( -0.000000000000000000, 1.000000000000000000, -0.000000000000000000 ) ) ;
#9720 = CIRCLE ( 'NONE', #7631, 50.00000000000000000 ) ;
#9722 = DIRECTION ( 'NONE',  ( -0.9945218953682744001, 0.1045284632676435205, 0.000000000000000000 ) ) ;
#9723 = AXIS2_PLACEMENT_3D ( 'NONE', #9329, #6767, #14380 ) ;
#9724 = CARTESIAN_POINT ( 'NONE',  ( -30.90169943749474513, 33.70000000000000284, -42.53254041760200721 ) ) ;
#9725 = LINE ( 'NONE', #3405, #15185 ) ;
#9726 = CARTESIAN_POINT ( 'NONE',  ( 40.45084971874737789, 44.58125000068280031, 29.38926261462365375 ) ) ;
#9727 = ORIENTED_EDGE ( 'NONE', *, *, #15135, .T. ) ;
#9728 = CARTESIAN_POINT ( 'NONE',  ( 30.81806926056962936, 31.15937500034139518, -42.41743335407647209 ) ) ;
#9729 = CARTESIAN_POINT ( 'NONE',  ( 0.000000000000000000, 262.0000000000000000, 0.000000000000000000 ) ) ;
#9730 = ORIENTED_EDGE ( 'NONE', *, *, #9870, .T. ) ;
#9731 = ORIENTED_EDGE ( 'NONE', *, *, #15309, .T. ) ;
#9732 = CARTESIAN_POINT ( 'NONE',  ( -3.219174618344376363E-15, 45.28125000068279604, -52.57311121191334990 ) ) ;
#9733 = VECTOR ( 'NONE', #4873, 1000.000000000000000 ) ;
#9734 = VECTOR ( 'NONE', #16157, 1000.000000000000000 ) ;
#9735 = AXIS2_PLACEMENT_3D ( 'NONE', #4341, #4182, #10734 ) ;
#9736 = FACE_OUTER_BOUND ( 'NONE', #9589, .T. ) ;
#9737 = FACE_BOUND ( 'NONE', #7154, .T. ) ;
#9738 = CIRCLE ( 'NONE', #1764, 45.00000000000000000 ) ;
#9739 = VERTEX_POINT ( 'NONE', #9955 ) ;
#9740 = LINE ( 'NONE', #15117, #16051 ) ;
#9741 = CARTESIAN_POINT ( 'NONE',  ( -7.919222016226804328, 28.22999571913594963, 50.00000000000000000 ) ) ;
#9742 = CYLINDRICAL_SURFACE ( 'NONE', #15021, 50.00000000000000000 ) ;
#9743 = CARTESIAN_POINT ( 'NONE',  ( 0.000000000000000000, 20.00000000000000355, 0.000000000000000000 ) ) ;
#9744 = DIRECTION ( 'NONE',  ( -0.000000000000000000, -1.000000000000000000, -0.000000000000000000 ) ) ;
#9745 = CARTESIAN_POINT ( 'NONE',  ( 0.000000000000000000, 280.0000000000000000, 0.000000000000000000 ) ) ;
#9746 = CARTESIAN_POINT ( 'NONE',  ( -50.00000000000000000, 32.00000000000000000, 0.000000000000000000 ) ) ;
#9747 = CARTESIAN_POINT ( 'NONE',  ( 15.45084971874737789, 36.38125000068279746, 47.55282581475767500 ) ) ;
#9748 = CARTESIAN_POINT ( 'NONE',  ( -15.45084971874737256, 41.60000000000000142, -47.55282581475767500 ) ) ;
#9749 = CARTESIAN_POINT ( 'NONE',  ( -49.86468353124999453, 23.82187500034139305, -16.20201782572375393 ) ) ;
#9750 = DIRECTION ( 'NONE',  ( -0.3090169943749573878, 0.9510565162951503115, 0.000000000000000000 ) ) ;
#9751 = CARTESIAN_POINT ( 'NONE',  ( -15.45084971874736368, 30.40000000000000213, 47.55282581475768211 ) ) ;
#9752 = CARTESIAN_POINT ( 'NONE',  ( 30.81806926056964002, 28.55937500034139731, 42.41743335407647209 ) ) ;
#9753 = LINE ( 'NONE', #11245, #1485 ) ;
#9754 = AXIS2_PLACEMENT_3D ( 'NONE', #9076, #6504, #1163 ) ;
#9755 = DIRECTION ( 'NONE',  ( 0.8090169943749426773, 0.5877852522924797984, 0.000000000000000000 ) ) ;
#9756 = ORIENTED_EDGE ( 'NONE', *, *, #11915, .F. ) ;
#9757 = CARTESIAN_POINT ( 'NONE',  ( 50.00000000000000000, 45.00000000000000711, -6.123233995736766085E-15 ) ) ;
#9758 = VERTEX_POINT ( 'NONE', #15011 ) ;
#9759 = CARTESIAN_POINT ( 'NONE',  ( 49.99999999999999289, 49.10000000000000142, -16.24598481164532160 ) ) ;
#9760 = CARTESIAN_POINT ( 'NONE',  ( 15.40903463028481113, 35.25937500034139305, -47.42413220539094709 ) ) ;
#9761 = DIRECTION ( 'NONE',  ( 0.000000000000000000, -0.000000000000000000, -1.000000000000000000 ) ) ;
#9762 = LINE ( 'NONE', #3604, #10176 ) ;
#9763 = AXIS2_PLACEMENT_3D ( 'NONE', #12695, #3884, #14010 ) ;
#9764 = DIRECTION ( 'NONE',  ( 0.000000000000000000, 0.000000000000000000, -1.000000000000000000 ) ) ;
#9765 = CARTESIAN_POINT ( 'NONE',  ( 40.34137639590981905, 32.72187500034139873, 29.30972558990010768 ) ) ;
#9766 = CARTESIAN_POINT ( 'NONE',  ( 49.86468353125001585, 28.75937500034139305, 16.20201782572375038 ) ) ;
#9767 = CARTESIAN_POINT ( 'NONE',  ( 7.919222016226809657, 27.22999571913595318, -50.00000000000000000 ) ) ;
#9768 = CARTESIAN_POINT ( 'NONE',  ( 15.40903463028481113, 27.32187500034139660, -47.42413220539094709 ) ) ;
#9769 = DIRECTION ( 'NONE',  ( 0.3213938048432687378, 0.5817472440052507965, 0.7471788047720987480 ) ) ;
#9770 = CARTESIAN_POINT ( 'NONE',  ( -49.86468353124999453, 47.75937500034139305, -16.20201782572375393 ) ) ;
#9771 = CARTESIAN_POINT ( 'NONE',  ( -30.81806926056963292, 37.62187500034139020, -42.41743335407647209 ) ) ;
#9772 = EDGE_CURVE ( 'NONE', #9937, #16264, #6718, .T. ) ;
#9773 = CARTESIAN_POINT ( 'NONE',  ( -15.40903463028480580, 20.32187500034139660, 47.42413220539094709 ) ) ;
#9775 = VERTEX_POINT ( 'NONE', #8025 ) ;
#9774 =( BOUNDED_CURVE ( )  B_SPLINE_CURVE ( 2, ( #11335, #3521, #7427, #12013, #13567, #4376, #13645 ),
 .UNSPECIFIED., .F., .F. ) 
 B_SPLINE_CURVE_WITH_KNOTS ( ( 3, 2, 2, 3 ),
 ( 0.000000000000000000, 0.006666666666666667095, 0.01333333333333333419, 0.01666666666666666644 ),
 .UNSPECIFIED. ) 
 CURVE ( )  GEOMETRIC_REPRESENTATION_ITEM ( )  RATIONAL_B_SPLINE_CURVE ( ( 1.000000000000000000, 0.9510565162951535312, 1.000000000000000000, 0.9510565162951535312, 1.000000000000000000, 0.9755282581475768211, 0.9755282581475768211 ) ) 
 REPRESENTATION_ITEM ( '' )  );
#9776 = CARTESIAN_POINT ( 'NONE',  ( -15.40903463028481646, 43.45937500034139589, -47.42413220539093999 ) ) ;
#9777 = VERTEX_POINT ( 'NONE', #9205 ) ;
#9779 = EDGE_CURVE ( 'NONE', #404, #10305, #1533, .T. ) ;
#9778 = CARTESIAN_POINT ( 'NONE',  ( 50.00000000000000000, 26.78125000068279959, -6.123233995736766085E-15 ) ) ;
#9780 = EDGE_CURVE ( 'NONE', #691, #2224, #9364, .T. ) ;
#9781 = ORIENTED_EDGE ( 'NONE', *, *, #15187, .F. ) ;
#9782 = EDGE_CURVE ( 'NONE', #1083, #1499, #4394, .T. ) ;
#9783 = CARTESIAN_POINT ( 'NONE',  ( -3.111920190527341144E-15, 35.50000000000000000, -50.00000000000000000 ) ) ;
#9784 = CARTESIAN_POINT ( 'NONE',  ( 15.40903463028482356, 38.52187500034139589, 47.42413220539093999 ) ) ;
#9785 = CARTESIAN_POINT ( 'NONE',  ( -49.86468353124999453, 21.75937500034140015, -16.20201782572375393 ) ) ;
#9786 = CARTESIAN_POINT ( 'NONE',  ( 49.99999999999999289, 41.10000000000000142, -16.24598481164532160 ) ) ;
#9787 = CARTESIAN_POINT ( 'NONE',  ( 15.40903463028482356, 22.52187500034139589, 47.42413220539093999 ) ) ;
#9788 = CARTESIAN_POINT ( 'NONE',  ( 49.99999999999999289, 32.88125000068280457, -16.24598481164532160 ) ) ;
#9789 = CARTESIAN_POINT ( 'NONE',  ( -15.40903463028481646, 37.52187500034139589, -47.42413220539093999 ) ) ;
#9790 = CARTESIAN_POINT ( 'NONE',  ( -25.66084200511936686, 284.4942466288902096, -3.821684010227674566 ) ) ;
#9791 = VERTEX_POINT ( 'NONE', #10621 ) ;
#9792 = CARTESIAN_POINT ( 'NONE',  ( -49.86468353125000164, 35.92187500034140157, 0.000000000000000000 ) ) ;
#9793 = CARTESIAN_POINT ( 'NONE',  ( -30.90169943749473447, 44.08125000068279320, 42.53254041760200721 ) ) ;
#9794 = ORIENTED_EDGE ( 'NONE', *, *, #11634, .T. ) ;
#9795 = ORIENTED_EDGE ( 'NONE', *, *, #7444, .T. ) ;
#9796 = ORIENTED_EDGE ( 'NONE', *, *, #9269, .T. ) ;
#9797 = DIRECTION ( 'NONE',  ( -0.000000000000000000, -0.000000000000000000, 1.000000000000000000 ) ) ;
#9798 = FACE_OUTER_BOUND ( 'NONE', #16280, .T. ) ;
#9799 = CARTESIAN_POINT ( 'NONE',  ( 0.000000000000000000, 20.00000000000000355, 0.000000000000000000 ) ) ;
#9800 = PLANE ( 'NONE',  #11368 ) ;
#9801 = CARTESIAN_POINT ( 'NONE',  ( 49.86468353125001585, 40.75937500034138594, 16.20201782572375038 ) ) ;
#9802 = DIRECTION ( 'NONE',  ( -0.3090169943749448977, -0.9510565162951543083, 0.000000000000000000 ) ) ;
#9803 = CARTESIAN_POINT ( 'NONE',  ( -25.00000000000000355, 307.0000000000000568, 7.500000000000001776 ) ) ;
#9804 = CARTESIAN_POINT ( 'NONE',  ( -2.267949192431125027, 22.50000000000000000, 100.0000000000000000 ) ) ;
#9805 =( LENGTH_UNIT ( ) NAMED_UNIT ( * ) SI_UNIT ( .MILLI., .METRE. ) );
#9806 = DIRECTION ( 'NONE',  ( 0.000000000000000000, 0.000000000000000000, -1.000000000000000000 ) ) ;
#9807 = PLANE ( 'NONE',  #7885 ) ;
#9808 = CARTESIAN_POINT ( 'NONE',  ( -49.99999999999999289, 34.10000000000000853, 16.24598481164533226 ) ) ;
#9809 = ORIENTED_EDGE ( 'NONE', *, *, #9568, .F. ) ;
#9810 = CARTESIAN_POINT ( 'NONE',  ( 40.34137639590981195, 33.05937500034139731, -29.30972558990011834 ) ) ;
#9811 = CARTESIAN_POINT ( 'NONE',  ( -3.111920190527341144E-15, 25.28125000068279604, -50.00000000000000000 ) ) ;
#9812 = ORIENTED_EDGE ( 'NONE', *, *, #8684, .F. ) ;
#9813 = ORIENTED_EDGE ( 'NONE', *, *, #10873, .F. ) ;
#9814 = CARTESIAN_POINT ( 'NONE',  ( 50.00000000000000000, 40.78125000068279604, -6.123233995736766085E-15 ) ) ;
#9815 = VECTOR ( 'NONE', #2058, 1000.000000000000114 ) ;
#9816 = CARTESIAN_POINT ( 'NONE',  ( 0.000000000000000000, 20.00000000000000355, 0.000000000000000000 ) ) ;
#9817 = CARTESIAN_POINT ( 'NONE',  ( 7.919222016226809657, 29.44874571845315359, -50.00000000000000000 ) ) ;
#9818 = ORIENTED_EDGE ( 'NONE', *, *, #5159, .T. ) ;
#9819 = CARTESIAN_POINT ( 'NONE',  ( 2.500000000000000000, 242.0000000000000284, -40.00000000000000000 ) ) ;
#9820 = CARTESIAN_POINT ( 'NONE',  ( -49.99999999999999289, 27.68125000068279462, -16.24598481164531449 ) ) ;
#9821 = CARTESIAN_POINT ( 'NONE',  ( -12.83488150441995401, 10.59022649794657234, 97.29057659180030271 ) ) ;
#9822 = DIRECTION ( 'NONE',  ( 0.000000000000000000, 0.000000000000000000, 1.000000000000000000 ) ) ;
#9823 = LINE ( 'NONE', #3329, #9123 ) ;
#9824 = CARTESIAN_POINT ( 'NONE',  ( 5.179451399591075145, 14.52044592729181538, 101.0000000000000000 ) ) ;
#9825 = CARTESIAN_POINT ( 'NONE',  ( 0.000000000000000000, 22.50000000000000000, 101.0000000000000000 ) ) ;
#9826 = ADVANCED_FACE ( 'NONE', ( #12945 ), #13187, .F. ) ;
#9827 = FACE_OUTER_BOUND ( 'NONE', #1026, .T. ) ;
#9828 = CARTESIAN_POINT ( 'NONE',  ( -45.93954244148126520, 20.00000000000000355, 19.39188242381481331 ) ) ;
#9829 = CARTESIAN_POINT ( 'NONE',  ( 9.657523855033129090E-15, 44.28125000068280315, 52.57311121191334990 ) ) ;
#9830 = LINE ( 'NONE', #12233, #13459 ) ;
#9831 = VECTOR ( 'NONE', #15276, 1000.000000000000000 ) ;
#9832 = CARTESIAN_POINT ( 'NONE',  ( -49.99999999999999289, 30.10000000000000497, 16.24598481164533226 ) ) ;
#9833 = CARTESIAN_POINT ( 'NONE',  ( -15.40903463028480580, 22.25937500034139660, 47.42413220539094709 ) ) ;
#9834 = CARTESIAN_POINT ( 'NONE',  ( 0.000000000000000000, 22.50000000000000000, 101.0000000000000000 ) ) ;
#9835 = DIRECTION ( 'NONE',  ( -0.000000000000000000, 0.000000000000000000, 1.000000000000000000 ) ) ;
#9836 = ORIENTED_EDGE ( 'NONE', *, *, #8085, .F. ) ;
#9837 = CARTESIAN_POINT ( 'NONE',  ( 7.919222016226809657, 45.44874571845314648, -50.00000000000000000 ) ) ;
#9838 = VERTEX_POINT ( 'NONE', #368 ) ;
#9839 = CARTESIAN_POINT ( 'NONE',  ( -1.688807283342575793, 101.8522485078275253, 9.657683769731228551 ) ) ;
#9840 = CARTESIAN_POINT ( 'NONE',  ( -30.81806926056962226, 36.15937500034139163, 42.41743335407647919 ) ) ;
#9841 = DIRECTION ( 'NONE',  ( 0.000000000000000000, 1.000000000000000000, 0.000000000000000000 ) ) ;
#9842 = FACE_OUTER_BOUND ( 'NONE', #8634, .T. ) ;
#9843 = CARTESIAN_POINT ( 'NONE',  ( 49.99999999999999289, 28.88125000068279391, -16.24598481164532160 ) ) ;
#9844 = DIRECTION ( 'NONE',  ( 1.000000000000000000, 0.000000000000000000, 0.000000000000000000 ) ) ;
#9845 = CARTESIAN_POINT ( 'NONE',  ( -3.210462471511496205E-15, 27.42187500034139092, -52.43083105670540789 ) ) ;
#9846 = CARTESIAN_POINT ( 'NONE',  ( -49.86468353124999453, 29.95937500034139589, 16.20201782572377169 ) ) ;
#9847 = CARTESIAN_POINT ( 'NONE',  ( 30.90169943749475223, 26.48125000068279888, 42.53254041760199300 ) ) ;
#9848 = CARTESIAN_POINT ( 'NONE',  ( -49.86468353124999453, 35.82187500034139305, -16.20201782572375393 ) ) ;
#9849 = CARTESIAN_POINT ( 'NONE',  ( -2.500000000000000000, 242.0000000000000284, -47.99999999999999289 ) ) ;
#9850 = CARTESIAN_POINT ( 'NONE',  ( -49.86468353125000164, 43.85937500034140157, 0.000000000000000000 ) ) ;
#9851 = CARTESIAN_POINT ( 'NONE',  ( 49.86468353125001585, 40.82187500034140726, 16.20201782572375038 ) ) ;
#9852 = CARTESIAN_POINT ( 'NONE',  ( 30.90169943749474157, 47.29999999999999716, -42.53254041760200721 ) ) ;
#9853 = ORIENTED_EDGE ( 'NONE', *, *, #8457, .T. ) ;
#9854 = CARTESIAN_POINT ( 'NONE',  ( 15.40903463028481113, 41.25937500034139305, -47.42413220539094709 ) ) ;
#9855 = EDGE_LOOP ( 'NONE', ( #8255, #14530, #13181 ) ) ;
#9856 = CARTESIAN_POINT ( 'NONE',  ( -49.99999999999999289, 23.68125000068279462, -16.24598481164531449 ) ) ;
#9857 = ORIENTED_EDGE ( 'NONE', *, *, #1002, .T. ) ;
#9858 = CARTESIAN_POINT ( 'NONE',  ( -10.69075041230567891, 8.636095224584611429, 101.0000000000000000 ) ) ;
#9859 = CARTESIAN_POINT ( 'NONE',  ( 15.40903463028482356, 48.52187500034140299, 47.42413220539093999 ) ) ;
#9860 = DIRECTION ( 'NONE',  ( 0.000000000000000000, 1.000000000000000000, 0.000000000000000000 ) ) ;
#9861 = CARTESIAN_POINT ( 'NONE',  ( 49.86468353125001585, 24.82187500034139305, 16.20201782572375038 ) ) ;
#9862 = CARTESIAN_POINT ( 'NONE',  ( -3.219174618344376363E-15, 31.28125000068279604, -52.57311121191334990 ) ) ;
#9863 = EDGE_CURVE ( 'NONE', #7784, #13965, #10448, .T. ) ;
#9864 =( BOUNDED_CURVE ( )  B_SPLINE_CURVE ( 2, ( #16108, #966, #5974, #2129, #12278, #14676, #12453 ),
 .UNSPECIFIED., .F., .F. ) 
 B_SPLINE_CURVE_WITH_KNOTS ( ( 3, 2, 2, 3 ),
 ( 0.000000000000000000, 0.006666666666666667095, 0.01333333333333333419, 0.01666666666666666644 ),
 .UNSPECIFIED. ) 
 CURVE ( )  GEOMETRIC_REPRESENTATION_ITEM ( )  RATIONAL_B_SPLINE_CURVE ( ( 1.000000000000000000, 0.9510565162951535312, 1.000000000000000000, 0.9510565162951535312, 1.000000000000000000, 0.9755282581475768211, 0.9755282581475768211 ) ) 
 REPRESENTATION_ITEM ( '' )  );
#9865 = CARTESIAN_POINT ( 'NONE',  ( 40.34137639590981195, 39.12187500034139731, -29.30972558990011834 ) ) ;
#9866 = CARTESIAN_POINT ( 'NONE',  ( -28.07127062163582920, 282.3184422169439927, -10.57127062163423403 ) ) ;
#9867 = EDGE_LOOP ( 'NONE', ( #3861, #9379, #4914, #6896 ) ) ;
#9868 = CARTESIAN_POINT ( 'NONE',  ( -3.210462471511496205E-15, 35.42187500034140157, -52.43083105670540789 ) ) ;
#9869 = CARTESIAN_POINT ( 'NONE',  ( -3.111920190527341144E-15, 43.28125000068280315, -50.00000000000000000 ) ) ;
#9870 = EDGE_CURVE ( 'NONE', #14534, #8275, #1791, .T. ) ;
#9871 = EDGE_LOOP ( 'NONE', ( #11806, #10182, #3409, #11247 ) ) ;
#9872 = ORIENTED_EDGE ( 'NONE', *, *, #12442, .T. ) ;
#9873 = ORIENTED_EDGE ( 'NONE', *, *, #3544, .F. ) ;
#9874 = FACE_OUTER_BOUND ( 'NONE', #3368, .T. ) ;
#9875 = CARTESIAN_POINT ( 'NONE',  ( -17.28626291527383785, 40.00000000000000711, 18.64048258526051427 ) ) ;
#9876 = ADVANCED_FACE ( 'NONE', ( #14092 ), #5315, .F. ) ;
#9877 = CARTESIAN_POINT ( 'NONE',  ( 8.446640517145639571E-15, 26.50000000000000000, 50.00000000000000000 ) ) ;
#9878 = FACE_OUTER_BOUND ( 'NONE', #1437, .T. ) ;
#9879 = CARTESIAN_POINT ( 'NONE',  ( -49.86468353124999453, 39.95937500034139589, 16.20201782572377525 ) ) ;
#9880 = CARTESIAN_POINT ( 'NONE',  ( -15.40903463028480580, 42.25937500034139305, 47.42413220539094709 ) ) ;
#9881 = CARTESIAN_POINT ( 'NONE',  ( 49.99999999999999289, 25.10000000000000142, -16.24598481164532160 ) ) ;
#9882 = CARTESIAN_POINT ( 'NONE',  ( -15.40903463028481646, 49.52187500034140299, -47.42413220539093999 ) ) ;
#9883 =( NAMED_UNIT ( * ) PLANE_ANGLE_UNIT ( ) SI_UNIT ( $, .RADIAN. ) );
#9884 = CARTESIAN_POINT ( 'NONE',  ( -49.95625437244530787, 20.00000000000000355, 4.103175251694850090 ) ) ;
#9885 = CARTESIAN_POINT ( 'NONE',  ( 50.00000000000000000, 42.78125000068280315, -6.123233995736766085E-15 ) ) ;
#9886 = CARTESIAN_POINT ( 'NONE',  ( 7.513064459987437071E-14, 42.50000000000000000, 50.00000000000000000 ) ) ;
#9887 = ORIENTED_EDGE ( 'NONE', *, *, #7951, .T. ) ;
#9888 = ADVANCED_FACE ( 'NONE', ( #11935 ), #6802, .T. ) ;
#9889 = CARTESIAN_POINT ( 'NONE',  ( -49.86468353125000164, 21.85937500034139802, 0.000000000000000000 ) ) ;
#9890 = ORIENTED_EDGE ( 'NONE', *, *, #6374, .F. ) ;
#9891 = ORIENTED_EDGE ( 'NONE', *, *, #9504, .T. ) ;
#9892 = EDGE_LOOP ( 'NONE', ( #8606, #16035, #981, #8973, #2803 ) ) ;
#9893 = CARTESIAN_POINT ( 'NONE',  ( 30.90169943749475578, 44.48125000068279888, 42.53254041760200010 ) ) ;
#9894 = CARTESIAN_POINT ( 'NONE',  ( 40.45084971874737789, 46.80000000000000426, 29.38926261462365375 ) ) ;
#9895 =( NAMED_UNIT ( * ) PLANE_ANGLE_UNIT ( ) SI_UNIT ( $, .RADIAN. ) );
#9896 = ADVANCED_FACE ( 'NONE', ( #5630 ), #10692, .T. ) ;
#9897 = ORIENTED_EDGE ( 'NONE', *, *, #14923, .F. ) ;
#9898 = CARTESIAN_POINT ( 'NONE',  ( -4.320770838041405604, 30.97531352606679178, 102.0000000000000142 ) ) ;
#9899 = FACE_OUTER_BOUND ( 'NONE', #15631, .T. ) ;
#9900 = CARTESIAN_POINT ( 'NONE',  ( -15.96758378294258662, 15.31621546249057708, 95.98047841688359938 ) ) ;
#9901 = DIRECTION ( 'NONE',  ( -0.000000000000000000, 1.000000000000000000, -0.000000000000000000 ) ) ;
#9902 = CARTESIAN_POINT ( 'NONE',  ( 48.35726954556789536, 24.99999999999999645, -12.16803787670825265 ) ) ;
#9903 = CARTESIAN_POINT ( 'NONE',  ( 41.19975849074683794, 25.00000000000000711, -28.55207485309309945 ) ) ;
#9905 = LINE ( 'NONE', #1553, #13194 ) ;
#9904 = AXIS2_PLACEMENT_3D ( 'NONE', #7044, #5570, #6893 ) ;
#9906 = CARTESIAN_POINT ( 'NONE',  ( -30.00000000000000711, 282.0000000000000000, -12.49999999999999822 ) ) ;
#9907 = CARTESIAN_POINT ( 'NONE',  ( 8.660254037844387298, 20.00000000000000355, 5.000000000000000000 ) ) ;
#9908 = CARTESIAN_POINT ( 'NONE',  ( -49.99999999999999289, 45.68125000068280173, -16.24598481164531449 ) ) ;
#9909 = CARTESIAN_POINT ( 'NONE',  ( 7.919222016226693306, 20.55125428154684641, 50.00000000000003553 ) ) ;
#9910 = CARTESIAN_POINT ( 'NONE',  ( 40.45084971874737079, 27.20000000000000284, -29.38926261462366440 ) ) ;
#9911 = CARTESIAN_POINT ( 'NONE',  ( -40.45084971874737079, 26.20000000000000284, 29.38926261462367151 ) ) ;
#9912 = EDGE_CURVE ( 'NONE', #5251, #2810, #12856, .T. ) ;
#9913 = CARTESIAN_POINT ( 'NONE',  ( -30.90169943749474513, 43.70000000000000284, -42.53254041760200721 ) ) ;
#9914 = CARTESIAN_POINT ( 'NONE',  ( 30.81806926056964002, 44.55937500034139020, 42.41743335407647209 ) ) ;
#9915 = ORIENTED_EDGE ( 'NONE', *, *, #15238, .T. ) ;
#9916 = CIRCLE ( 'NONE', #13896, 17.50000000000000000 ) ;
#9917 = CARTESIAN_POINT ( 'NONE',  ( 15.45084971874737789, 44.60000000000000142, 47.55282581475767500 ) ) ;
#9918 = ORIENTED_EDGE ( 'NONE', *, *, #3110, .T. ) ;
#9919 = CARTESIAN_POINT ( 'NONE',  ( 0.000000000000000000, 217.0000000000000284, 40.00000000000000000 ) ) ;
#9920 = CARTESIAN_POINT ( 'NONE',  ( -49.86468353124999453, 37.75937500034140015, -16.20201782572375393 ) ) ;
#9921 = CARTESIAN_POINT ( 'NONE',  ( 40.45084971874737079, 40.98125000068279888, -29.38926261462366440 ) ) ;
#9922 = DIRECTION ( 'NONE',  ( 0.000000000000000000, 0.000000000000000000, -1.000000000000000000 ) ) ;
#9923 = CARTESIAN_POINT ( 'NONE',  ( 7.919222016226693306, 34.55125428154684641, 50.00000000000003553 ) ) ;
#9924 = CARTESIAN_POINT ( 'NONE',  ( 8.660254037844387298, 25.00000000000000355, 5.000000000000000000 ) ) ;
#9925 = CARTESIAN_POINT ( 'NONE',  ( -49.86468353124999453, 26.02187500034139944, 16.20201782572377525 ) ) ;
#9926 = CARTESIAN_POINT ( 'NONE',  ( 49.86468353125001585, 32.75937500034140015, 16.20201782572375038 ) ) ;
#9927 = CARTESIAN_POINT ( 'NONE',  ( 9.642970592016647302, 99.14870971539799882, -1.872989114519519882 ) ) ;
#9928 = CARTESIAN_POINT ( 'NONE',  ( 49.86468353124999453, 33.02187500034139589, -16.20201782572376104 ) ) ;
#9929 = CARTESIAN_POINT ( 'NONE',  ( -20.00000000000000355, 307.0000000000000568, 2.500000000000001332 ) ) ;
#9930 = AXIS2_PLACEMENT_3D ( 'NONE', #392, #4067, #5499 ) ;
#9931 = CARTESIAN_POINT ( 'NONE',  ( 40.34137639590981195, 37.05937500034139731, -29.30972558990011834 ) ) ;
#9932 = CARTESIAN_POINT ( 'NONE',  ( 9.631387414534489405E-15, 38.42187500034139447, 52.43083105670540789 ) ) ;
#9933 = CARTESIAN_POINT ( 'NONE',  ( -49.99999999999999289, 48.10000000000000142, 16.24598481164533226 ) ) ;
#9934 = EDGE_LOOP ( 'NONE', ( #77, #2126, #13356, #12955 ) ) ;
#9935 = CARTESIAN_POINT ( 'NONE',  ( 40.34137639590981905, 42.65937500034139873, 29.30972558990010768 ) ) ;
#9936 = EDGE_CURVE ( 'NONE', #14188, #3704, #10539, .T. ) ;
#9937 = VERTEX_POINT ( 'NONE', #15599 ) ;
#9938 = CARTESIAN_POINT ( 'NONE',  ( -3.219174618344376363E-15, 21.28125000068279959, -52.57311121191334990 ) ) ;
#9939 = PLANE ( 'NONE',  #16314 ) ;
#9940 = CARTESIAN_POINT ( 'NONE',  ( -40.45084971874737079, 36.20000000000000284, 29.38926261462367151 ) ) ;
#9941 = CARTESIAN_POINT ( 'NONE',  ( -30.81806926056963292, 41.62187500034139020, -42.41743335407647209 ) ) ;
#9942 = DIRECTION ( 'NONE',  ( -0.000000000000000000, 1.000000000000000000, -0.000000000000000000 ) ) ;
#9943 = CARTESIAN_POINT ( 'NONE',  ( 49.86468353124999453, 21.02187500034139589, -16.20201782572376459 ) ) ;
#9944 = CARTESIAN_POINT ( 'NONE',  ( 15.45084971874736723, 29.18125000068279817, -47.55282581475768211 ) ) ;
#9945 = VECTOR ( 'NONE', #9098, 1000.000000000000000 ) ;
#9946 = CARTESIAN_POINT ( 'NONE',  ( 49.86468353125001585, 32.82187500034139305, 16.20201782572375038 ) ) ;
#9947 = CARTESIAN_POINT ( 'NONE',  ( -20.51073895446497986, 285.3889217077648368, -7.755369477226732755 ) ) ;
#9948 = CARTESIAN_POINT ( 'NONE',  ( 30.81806926056962936, 35.22187500034138452, -42.41743335407647209 ) ) ;
#9949 = CARTESIAN_POINT ( 'NONE',  ( -30.90169943749473447, 42.08125000068279320, 42.53254041760200721 ) ) ;
#9950 = EDGE_LOOP ( 'NONE', ( #15378, #11558 ) ) ;
#9951 = ORIENTED_EDGE ( 'NONE', *, *, #8837, .F. ) ;
#9952 = ORIENTED_EDGE ( 'NONE', *, *, #4314, .T. ) ;
#9953 = EDGE_CURVE ( 'NONE', #8347, #7069, #290, .T. ) ;
#9954 = CARTESIAN_POINT ( 'NONE',  ( 1.490838860747792127E-14, 45.00000000000002132, 44.99999999999998579 ) ) ;
#9955 = CARTESIAN_POINT ( 'NONE',  ( 7.977241335952203194, 17.31698729810786475, 102.0000000000000142 ) ) ;
#9956 = AXIS2_PLACEMENT_3D ( 'NONE', #1065, #13378, #899 ) ;
#9957 = DIRECTION ( 'NONE',  ( 0.000000000000000000, -0.000000000000000000, 1.000000000000000000 ) ) ;
#9958 = CARTESIAN_POINT ( 'NONE',  ( -30.90169943749473447, 24.08125000068279675, 42.53254041760200721 ) ) ;
#9959 = CARTESIAN_POINT ( 'NONE',  ( 40.34137639590981905, 30.65937500034139518, 29.30972558990010768 ) ) ;
#9960 = CARTESIAN_POINT ( 'NONE',  ( 30.81806926056964002, 40.55937500034139731, 42.41743335407646498 ) ) ;
#9961 =( BOUNDED_CURVE ( )  B_SPLINE_CURVE ( 2, ( #7114, #14816, #12170, #12426, #5946, #771, #11008, #4706, #3447, #12331, #932, #15146, #14064 ),
 .UNSPECIFIED., .F., .F. ) 
 B_SPLINE_CURVE_WITH_KNOTS ( ( 3, 2, 2, 2, 2, 2, 3 ),
 ( 0.5500000000000000444, 0.5533333333333333437, 0.5600000000000000533, 0.5666666666666666519, 0.5733333333333333615, 0.5799999999999999600, 0.5833333333333333703 ),
 .UNSPECIFIED. ) 
 CURVE ( )  GEOMETRIC_REPRESENTATION_ITEM ( )  RATIONAL_B_SPLINE_CURVE ( ( 0.9755282581475768211, 0.9755282581475771542, 1.000000000000000000, 0.9510565162951535312, 1.000000000000000000, 0.9510565162951535312, 1.000000000000000000, 0.9510565162951535312, 1.000000000000000000, 0.9510565162951535312, 1.000000000000000000, 0.9755282581475763770, 0.9755282581475768211 ) ) 
 REPRESENTATION_ITEM ( '' )  );
#9962 = LINE ( 'NONE', #10959, #15578 ) ;
#9963 = LINE ( 'NONE', #13693, #373 ) ;
#9964 = FACE_OUTER_BOUND ( 'NONE', #3048, .T. ) ;
#9965 = CARTESIAN_POINT ( 'NONE',  ( 29.32979127811506004, 25.09142360399907901, -43.04328433925368813 ) ) ;
#9966 = ORIENTED_EDGE ( 'NONE', *, *, #14122, .F. ) ;
#9967 = AXIS2_PLACEMENT_3D ( 'NONE', #2902, #13042, #802 ) ;
#9968 = ADVANCED_FACE ( 'NONE', ( #9287, #11615 ), #10366, .F. ) ;
#9969 = CARTESIAN_POINT ( 'NONE',  ( 49.86468353125000164, 26.85937500034139802, -6.106662507704105588E-15 ) ) ;
#9970 = ORIENTED_EDGE ( 'NONE', *, *, #11292, .T. ) ;
#9971 = ORIENTED_EDGE ( 'NONE', *, *, #14934, .F. ) ;
#9972 = ORIENTED_EDGE ( 'NONE', *, *, #1682, .F. ) ;
#9973 = PRESENTATION_LAYER_ASSIGNMENT (  '', '', ( #3875 ) ) ;
#9974 = ADVANCED_FACE ( 'NONE', ( #15425, #4045 ), #9115, .T. ) ;
#9975 = CARTESIAN_POINT ( 'NONE',  ( 40.45084971874737079, 38.98125000068279888, -29.38926261462366440 ) ) ;
#9976 = CARTESIAN_POINT ( 'NONE',  ( 6.123233995736766085E-15, 193.4213562373095385, 50.00000000000000000 ) ) ;
#9977 = LINE ( 'NONE', #3906, #5463 ) ;
#9978 = VERTEX_POINT ( 'NONE', #612 ) ;
#9979 = CARTESIAN_POINT ( 'NONE',  ( 15.45084971874736723, 39.18125000068280173, -47.55282581475768211 ) ) ;
#9980 = CYLINDRICAL_SURFACE ( 'NONE', #12202, 50.00000000000000000 ) ;
#9981 = DIRECTION ( 'NONE',  ( 0.000000000000000000, 0.000000000000000000, 1.000000000000000000 ) ) ;
#9982 = CARTESIAN_POINT ( 'NONE',  ( 1.671572875253809487, 246.1715728752537871, 50.00000000000000000 ) ) ;
#9983 = VECTOR ( 'NONE', #44, 1000.000000000000000 ) ;
#9984 = DIRECTION ( 'NONE',  ( 0.000000000000000000, 0.000000000000000000, -1.000000000000000000 ) ) ;
#9985 = DIRECTION ( 'NONE',  ( 1.000000000000000000, 0.000000000000000000, 0.000000000000000000 ) ) ;
#9986 = CIRCLE ( 'NONE', #12095, 17.50000000000000000 ) ;
#9987 = FACE_OUTER_BOUND ( 'NONE', #6973, .T. ) ;
#9988 = EDGE_CURVE ( 'NONE', #7989, #2880, #14739, .T. ) ;
#9989 = LINE ( 'NONE', #6246, #14694 ) ;
#9990 = CARTESIAN_POINT ( 'NONE',  ( -50.00000000000000000, 45.78125000068279604, 0.000000000000000000 ) ) ;
#9991 = CARTESIAN_POINT ( 'NONE',  ( -49.99999999999999289, 26.10000000000000142, 16.24598481164533226 ) ) ;
#9992 = CARTESIAN_POINT ( 'NONE',  ( 9.631387414534489405E-15, 22.35937500034139802, 52.43083105670540789 ) ) ;
#9993 = CARTESIAN_POINT ( 'NONE',  ( -7.580410092413954359, 99.32916037694960210, 5.000000000000000000 ) ) ;
#9994 = CARTESIAN_POINT ( 'NONE',  ( 9.631387414534489405E-15, 44.35937500034140157, 52.43083105670540789 ) ) ;
#9995 = TOROIDAL_SURFACE ( 'NONE', #15563, 7.732050807568878525, 2.000000000000000000 ) ;
#9996 = EDGE_LOOP ( 'NONE', ( #8601, #6227, #6103, #10706 ) ) ;
#9997 = VECTOR ( 'NONE', #14544, 1000.000000000000000 ) ;
#9998 = AXIS2_PLACEMENT_3D ( 'NONE', #5357, #12985, #15467 ) ;
#9999 = AXIS2_PLACEMENT_3D ( 'NONE', #15369, #14038, #9062 ) ;
#10000 = CARTESIAN_POINT ( 'NONE',  ( 15.45084971874736723, 43.18125000068280173, -47.55282581475768211 ) ) ;
#10001 = VERTEX_POINT ( 'NONE', #12419 ) ;
#10002 = DIRECTION ( 'NONE',  ( 0.000000000000000000, 0.000000000000000000, -1.000000000000000000 ) ) ;
#10003 = CARTESIAN_POINT ( 'NONE',  ( -49.86468353125000164, 33.85937500034139447, 0.000000000000000000 ) ) ;
#10004 = CARTESIAN_POINT ( 'NONE',  ( 0.000000000000000000, 193.4213562373095385, 0.000000000000000000 ) ) ;
#10005 = DIRECTION ( 'NONE',  ( 1.000000000000000000, -2.577303450022684939E-15, 0.000000000000000000 ) ) ;
#10006 = EDGE_CURVE ( 'NONE', #1819, #12542, #6107, .T. ) ;
#10007 = CARTESIAN_POINT ( 'NONE',  ( 45.87472660798608359, 24.99999999999998579, -19.54543171153504488 ) ) ;
#10008 = DIRECTION ( 'NONE',  ( 0.000000000000000000, 1.000000000000000000, 0.000000000000000000 ) ) ;
#10009 = CIRCLE ( 'NONE', #4715, 60.00000000000000711 ) ;
#10010 = CARTESIAN_POINT ( 'NONE',  ( -30.81806926056963292, 25.62187500034139731, -42.41743335407647209 ) ) ;
#10011 = CARTESIAN_POINT ( 'NONE',  ( 40.34137639590981905, 20.65937500034139873, 29.30972558990010768 ) ) ;
#10012 = AXIS2_PLACEMENT_3D ( 'NONE', #6415, #12647, #4774 ) ;
#10013 = CARTESIAN_POINT ( 'NONE',  ( 15.45084971874737789, 42.60000000000000142, 47.55282581475767500 ) ) ;
#10014 = CARTESIAN_POINT ( 'NONE',  ( -15.40903463028480580, 36.32187500034140015, 47.42413220539094709 ) ) ;
#10015 = AXIS2_PLACEMENT_3D ( 'NONE', #2668, #1506, #248 ) ;
#10016 = CARTESIAN_POINT ( 'NONE',  ( -50.00000000000000000, 29.78125000068279959, 0.000000000000000000 ) ) ;
#10017 = CARTESIAN_POINT ( 'NONE',  ( -40.45084971874737789, 35.79999999999999716, -29.38926261462365730 ) ) ;
#10018 = CARTESIAN_POINT ( 'NONE',  ( 49.86468353124999453, 40.95937500034140299, -16.20201782572376459 ) ) ;
#10019 = CARTESIAN_POINT ( 'NONE',  ( 40.34137639590981195, 29.12187500034139376, -29.30972558990011834 ) ) ;
#10020 =( BOUNDED_CURVE ( )  B_SPLINE_CURVE ( 2, ( #11161, #5758, #5838, #9652, #13385, #4675, #7332, #8320, #993, #3586, #9747, #12149, #2330 ),
 .UNSPECIFIED., .F., .F. ) 
 B_SPLINE_CURVE_WITH_KNOTS ( ( 3, 2, 2, 2, 2, 2, 3 ),
 ( 0.4166666666666666852, 0.4199999999999999845, 0.4266666666666666941, 0.4333333333333333481, 0.4400000000000000022, 0.4466666666666666563, 0.4500000000000000111 ),
 .UNSPECIFIED. ) 
 CURVE ( )  GEOMETRIC_REPRESENTATION_ITEM ( )  RATIONAL_B_SPLINE_CURVE ( ( 0.9755282581475768211, 0.9755282581475770431, 1.000000000000000000, 0.9510565162951535312, 1.000000000000000000, 0.9510565162951535312, 1.000000000000000000, 0.9510565162951535312, 1.000000000000000000, 0.9510565162951535312, 1.000000000000000000, 0.9755282581475765991, 0.9755282581475768211 ) ) 
 REPRESENTATION_ITEM ( '' )  );
#10021 = CARTESIAN_POINT ( 'NONE',  ( -49.99999999999999289, 44.09999999999999432, 16.24598481164533226 ) ) ;
#10022 = EDGE_LOOP ( 'NONE', ( #9421, #2145, #5995, #1545 ) ) ;
#10023 = CARTESIAN_POINT ( 'NONE',  ( -15.40903463028480580, 40.25937500034139305, 47.42413220539094709 ) ) ;
#10024 = CONICAL_SURFACE ( 'NONE', #3105, 16.50000000000000711, 0.7853981633974447263 ) ;
#10025 = ORIENTED_EDGE ( 'NONE', *, *, #12949, .F. ) ;
#10026 = VERTEX_POINT ( 'NONE', #15063 ) ;
#10028 = CARTESIAN_POINT ( 'NONE',  ( 40.45084971874737789, 26.58125000068279675, 29.38926261462365375 ) ) ;
#10027 = VECTOR ( 'NONE', #4922, 1000.000000000000114 ) ;
#10029 = LINE ( 'NONE', #105, #13648 ) ;
#10030 = CARTESIAN_POINT ( 'NONE',  ( 30.81806926056964002, 22.62187500034139731, 42.41743335407647209 ) ) ;
#10031 = FACE_BOUND ( 'NONE', #9950, .T. ) ;
#10032 = CARTESIAN_POINT ( 'NONE',  ( 30.81806926056962936, 39.22187500034139873, -42.41743335407647209 ) ) ;
#10033 = EDGE_CURVE ( 'NONE', #12541, #40, #12496, .T. ) ;
#10034 = CARTESIAN_POINT ( 'NONE',  ( 49.99999999999999289, 49.10000000000000853, -16.24598481164532160 ) ) ;
#10035 = ADVANCED_FACE ( 'NONE', ( #6181 ), #16232, .F. ) ;
#10036 = CARTESIAN_POINT ( 'NONE',  ( 50.00000000000000000, 28.78125000068279959, -6.123233995736766085E-15 ) ) ;
#10037 = CARTESIAN_POINT ( 'NONE',  ( 40.34137639590981195, 35.12187500034139731, -29.30972558990011834 ) ) ;
#10038 = CARTESIAN_POINT ( 'NONE',  ( -28.69101924422432148, 282.0322304394514390, -11.84550962211183389 ) ) ;
#10039 = CARTESIAN_POINT ( 'NONE',  ( 15.40903463028481113, 37.32187500034140015, -47.42413220539094709 ) ) ;
#10040 = CARTESIAN_POINT ( 'NONE',  ( -0.5000000000000000000, 39.99999999999999289, 102.0000000000000142 ) ) ;
#10041 = ORIENTED_EDGE ( 'NONE', *, *, #13093, .T. ) ;
#10042 = VERTEX_POINT ( 'NONE', #5708 ) ;
#10043 = PLANE ( 'NONE',  #9763 ) ;
#10044 = CARTESIAN_POINT ( 'NONE',  ( -2.500000000000000000, 242.0000000000000284, -44.93050188902856945 ) ) ;
#10045 = CARTESIAN_POINT ( 'NONE',  ( -40.45084971874737079, 24.20000000000000284, 29.38926261462367151 ) ) ;
#10046 = DIRECTION ( 'NONE',  ( 0.000000000000000000, 0.000000000000000000, 1.000000000000000000 ) ) ;
#10047 = CARTESIAN_POINT ( 'NONE',  ( -3.210462471511496205E-15, 29.35937500034139802, -52.43083105670540789 ) ) ;
#10048 = DIRECTION ( 'NONE',  ( 0.000000000000000000, -1.000000000000000000, 0.000000000000000000 ) ) ;
#10049 = CARTESIAN_POINT ( 'NONE',  ( 15.40903463028482356, 46.52187500034139589, 47.42413220539093999 ) ) ;
#10050 = VECTOR ( 'NONE', #16439, 1000.000000000000000 ) ;
#10051 = CARTESIAN_POINT ( 'NONE',  ( 0.000000000000000000, 272.0000000000000000, 0.000000000000000000 ) ) ;
#10052 = CARTESIAN_POINT ( 'NONE',  ( 9.500222237632415911, 22.00424054664152607, 101.0000000000000000 ) ) ;
#10053 = APPLICATION_CONTEXT ( 'automotive_design' ) ;
#10054 = ORIENTED_EDGE ( 'NONE', *, *, #11726, .F. ) ;
#10055 = CARTESIAN_POINT ( 'NONE',  ( 30.81806926056962936, 27.15937500034139163, -42.41743335407647209 ) ) ;
#10056 = EDGE_LOOP ( 'NONE', ( #11914, #9399, #11521, #9970, #9493 ) ) ;
#10057 = ORIENTED_EDGE ( 'NONE', *, *, #15858, .F. ) ;
#10058 = ORIENTED_EDGE ( 'NONE', *, *, #11093, .F. ) ;
#10059 = VERTEX_POINT ( 'NONE', #4866 ) ;
#10060 = FACE_OUTER_BOUND ( 'NONE', #2809, .T. ) ;
#10061 = PLANE ( 'NONE',  #9436 ) ;
#10062 = ORIENTED_EDGE ( 'NONE', *, *, #1214, .T. ) ;
#10063 = DIRECTION ( 'NONE',  ( 0.000000000000000000, 0.7071067811865463515, -0.7071067811865487940 ) ) ;
#10064 = CARTESIAN_POINT ( 'NONE',  ( 5.000000000000000000, 0.000000000000000000, 0.000000000000000000 ) ) ;
#10065 = CARTESIAN_POINT ( 'NONE',  ( 7.919222016226693306, 32.33250428222964246, 50.00000000000003553 ) ) ;
#10066 = DIRECTION ( 'NONE',  ( 0.000000000000000000, 1.541976423090494894E-16, 1.000000000000000000 ) ) ;
#10067 = DIRECTION ( 'NONE',  ( 0.7071067811865484609, -0.7071067811865465735, -2.453269466693401579E-16 ) ) ;
#10068 = CARTESIAN_POINT ( 'NONE',  ( 1.875620865444973696E-15, 37.00000000000001421, -3.248670634687016947E-15 ) ) ;
#10069 = ADVANCED_FACE ( 'NONE', ( #14975 ), #8746, .F. ) ;
#10070 = CARTESIAN_POINT ( 'NONE',  ( 1.105645237078933619E-14, 92.00000000000001421, 14.08089297201389378 ) ) ;
#10071 = DIRECTION ( 'NONE',  ( 0.000000000000000000, 1.000000000000000000, 0.000000000000000000 ) ) ;
#10072 = CARTESIAN_POINT ( 'NONE',  ( -15.45084971874737256, 45.38125000068279746, -47.55282581475767500 ) ) ;
#10073 = CARTESIAN_POINT ( 'NONE',  ( -30.27664397204038593, 40.00000000000000711, 26.14048258526057467 ) ) ;
#10074 = CARTESIAN_POINT ( 'NONE',  ( 9.657523855033129090E-15, 20.50000000000000355, 52.57311121191334990 ) ) ;
#10075 = CARTESIAN_POINT ( 'NONE',  ( 15.40903463028481113, 21.25937500034139660, -47.42413220539094709 ) ) ;
#10076 = CARTESIAN_POINT ( 'NONE',  ( 1.010305842943185372E-14, 272.0000000000000000, 82.49773270518484480 ) ) ;
#10077 = EDGE_CURVE ( 'NONE', #1042, #12043, #1473, .T. ) ;
#10078 = CARTESIAN_POINT ( 'NONE',  ( 9.631387414534489405E-15, 42.35937500034140157, 52.43083105670540789 ) ) ;
#10079 = COLOUR_RGB ( '', 0.66274510, 0.83137255, 0.94901961) ;
#10080 = ORIENTED_EDGE ( 'NONE', *, *, #6005, .T. ) ;
#10081 = FILL_AREA_STYLE ('',( #14129 ) ) ;
#10082 = EDGE_CURVE ( 'NONE', #14108, #5931, #9986, .T. ) ;
#10083 = ORIENTED_EDGE ( 'NONE', *, *, #1684, .T. ) ;
#10084 = DIRECTION ( 'NONE',  ( 0.2079116908177531253, 0.9781476007338069101, 0.000000000000000000 ) ) ;
#10085 = CARTESIAN_POINT ( 'NONE',  ( -40.34137639590981905, 27.65937500034139873, -29.30972558990011478 ) ) ;
#10086 = CARTESIAN_POINT ( 'NONE',  ( -36.11321354817288665, 35.02991267065632286, -17.92868204048059155 ) ) ;
#10087 = DIRECTION ( 'NONE',  ( 0.9510565162951544194, -0.3090169943749448422, 0.000000000000000000 ) ) ;
#10088 = CARTESIAN_POINT ( 'NONE',  ( 45.47188453826132104, 25.00000000000000000, -20.46517872429543061 ) ) ;
#10089 = CARTESIAN_POINT ( 'NONE',  ( -40.34137639590981195, 34.12187500034139731, 29.30972558990012189 ) ) ;
#10090 = ADVANCED_FACE ( 'NONE', ( #9842 ), #8198, .F. ) ;
#10091 = CARTESIAN_POINT ( 'NONE',  ( 8.679606986189813260E-15, 55.00000000000000711, -62.25100647794772613 ) ) ;
#10092 = VECTOR ( 'NONE', #3667, 1000.000000000000000 ) ;
#10093 = CARTESIAN_POINT ( 'NONE',  ( -49.86468353125000164, 25.92187500034139802, 0.000000000000000000 ) ) ;
#10094 = CARTESIAN_POINT ( 'NONE',  ( -49.86468353125000164, 21.85937500034139802, 0.000000000000000000 ) ) ;
#10095 = CARTESIAN_POINT ( 'NONE',  ( 49.86468353125001585, 32.82187500034139305, 16.20201782572375038 ) ) ;
#10096 = CARTESIAN_POINT ( 'NONE',  ( 0.000000000000000000, 20.00000000000000355, 50.00000000000000000 ) ) ;
#10097 = CARTESIAN_POINT ( 'NONE',  ( 30.90169943749474157, 31.30000000000000071, -42.53254041760200721 ) ) ;
#10098 = CARTESIAN_POINT ( 'NONE',  ( -30.81806926056962226, 38.15937500034138452, 42.41743335407647919 ) ) ;
#10099 = CARTESIAN_POINT ( 'NONE',  ( 15.40903463028482356, 28.52187500034139589, 47.42413220539093999 ) ) ;
#10100 = CARTESIAN_POINT ( 'NONE',  ( 40.45084971874737789, 46.80000000000000426, 29.38926261462365375 ) ) ;
#10101 = ORIENTED_EDGE ( 'NONE', *, *, #11569, .F. ) ;
#10102 = CARTESIAN_POINT ( 'NONE',  ( -15.40903463028481646, 35.45937500034139589, -47.42413220539093999 ) ) ;
#10103 = ORIENTED_EDGE ( 'NONE', *, *, #5847, .F. ) ;
#10104 = ORIENTED_EDGE ( 'NONE', *, *, #4039, .F. ) ;
#10105 = CARTESIAN_POINT ( 'NONE',  ( 20.00000000000000355, 287.0000000000000568, -7.500000000000000888 ) ) ;
#10106 = CARTESIAN_POINT ( 'NONE',  ( 15.45084971874737789, 20.38125000068279746, 47.55282581475767500 ) ) ;
#10107 = CARTESIAN_POINT ( 'NONE',  ( -30.90169943749474513, 33.70000000000000284, -42.53254041760200721 ) ) ;
#10108 = CARTESIAN_POINT ( 'NONE',  ( 40.34137639590981195, 23.12187500034139731, -29.30972558990011834 ) ) ;
#10109 = EDGE_CURVE ( 'NONE', #243, #8698, #4466, .T. ) ;
#10110 = CARTESIAN_POINT ( 'NONE',  ( -5.000000000000000000, 32.40304740096967606, 41.61750739262920717 ) ) ;
#10111 = CARTESIAN_POINT ( 'NONE',  ( 15.40903463028481113, 41.32187500034140015, -47.42413220539094709 ) ) ;
#10112 = CARTESIAN_POINT ( 'NONE',  ( 2.500000000000000000, 244.0000000000000284, 49.99999999999999289 ) ) ;
#10113 = SHAPE_REPRESENTATION ( 'cutter assembly', ( #15812 ), #3617 ) ;
#10114 = CARTESIAN_POINT ( 'NONE',  ( 50.00000000000000000, 49.00000000000000000, -6.123233995736766085E-15 ) ) ;
#10115 = CARTESIAN_POINT ( 'NONE',  ( -30.90169943749473802, 30.08125000068279675, 42.53254041760200721 ) ) ;
#10116 = CARTESIAN_POINT ( 'NONE',  ( -40.34137639590981195, 48.12187500034139731, 29.30972558990012189 ) ) ;
#10117 = CARTESIAN_POINT ( 'NONE',  ( -40.34137639590981905, 31.72187500034139873, -29.30972558990011478 ) ) ;
#10118 = CARTESIAN_POINT ( 'NONE',  ( 15.45084971874737789, 38.60000000000000142, 47.55282581475767500 ) ) ;
#10119 = FACE_OUTER_BOUND ( 'NONE', #2222, .T. ) ;
#10120 = ORIENTED_EDGE ( 'NONE', *, *, #10664, .T. ) ;
#10121 = ORIENTED_EDGE ( 'NONE', *, *, #1424, .F. ) ;
#10122 = EDGE_CURVE ( 'NONE', #6731, #4841, #2422, .T. ) ;
#10123 = DIRECTION ( 'NONE',  ( 0.000000000000000000, 0.000000000000000000, -1.000000000000000000 ) ) ;
#10124 = CARTESIAN_POINT ( 'NONE',  ( 15.45084971874737789, 44.60000000000000142, 47.55282581475767500 ) ) ;
#10125 = CARTESIAN_POINT ( 'NONE',  ( -2.267949192431125027, 22.50000000000000000, 102.0000000000000142 ) ) ;
#10126 = LINE ( 'NONE', #8958, #11643 ) ;
#10127 = CARTESIAN_POINT ( 'NONE',  ( 15.40903463028482356, 28.45937500034139589, 47.42413220539093999 ) ) ;
#10128 = DIRECTION ( 'NONE',  ( -1.156482317317871478E-16, 0.000000000000000000, -1.000000000000000000 ) ) ;
#10129 = CARTESIAN_POINT ( 'NONE',  ( 49.86468353125000164, 46.92187500034139447, -6.106662507704105588E-15 ) ) ;
#10130 = FACE_OUTER_BOUND ( 'NONE', #13805, .T. ) ;
#10131 = DIRECTION ( 'NONE',  ( 0.000000000000000000, 0.000000000000000000, 1.000000000000000000 ) ) ;
#10132 = CARTESIAN_POINT ( 'NONE',  ( -15.45084971874736368, 42.39999999999999858, 47.55282581475768211 ) ) ;
#10133 = ORIENTED_EDGE ( 'NONE', *, *, #12196, .F. ) ;
#10134 = CARTESIAN_POINT ( 'NONE',  ( 15.40903463028482356, 24.45937500034139589, 47.42413220539093999 ) ) ;
#10135 = ORIENTED_EDGE ( 'NONE', *, *, #10357, .F. ) ;
#10136 = CARTESIAN_POINT ( 'NONE',  ( 0.000000000000000000, 52.00000000000000711, 0.000000000000000000 ) ) ;
#10137 = EDGE_LOOP ( 'NONE', ( #3046, #12256, #3737, #3314 ) ) ;
#10138 = EDGE_LOOP ( 'NONE', ( #11538, #11968 ) ) ;
#10139 = CARTESIAN_POINT ( 'NONE',  ( 40.45084971874737789, 34.58125000068280031, 29.38926261462365375 ) ) ;
#10140 = CARTESIAN_POINT ( 'NONE',  ( 37.77664397204061686, 40.00000000000000711, 13.15010152849349900 ) ) ;
#10141 = CARTESIAN_POINT ( 'NONE',  ( -15.45084971874737256, 27.60000000000000142, -47.55282581475767500 ) ) ;
#10142 = CARTESIAN_POINT ( 'NONE',  ( 7.977241335952203194, 17.31698729810786475, 101.0000000000000000 ) ) ;
#10143 = CARTESIAN_POINT ( 'NONE',  ( 0.000000000000000000, 51.99999999999999289, -50.00000000000000000 ) ) ;
#10144 = CARTESIAN_POINT ( 'NONE',  ( 4.127528389677815213, 5.486372832567310454, 101.0000000000000000 ) ) ;
#10145 = CARTESIAN_POINT ( 'NONE',  ( -9.881733417930727015, 8.048309972292139847, 101.0000000000000000 ) ) ;
#10146 = CARTESIAN_POINT ( 'NONE',  ( 0.000000000000000000, 25.00000000000000355, 0.000000000000000000 ) ) ;
#10147 =( LENGTH_UNIT ( ) NAMED_UNIT ( * ) SI_UNIT ( .MILLI., .METRE. ) );
#10148 = DIRECTION ( 'NONE',  ( 0.000000000000000000, 1.000000000000000000, 0.000000000000000000 ) ) ;
#10149 = CARTESIAN_POINT ( 'NONE',  ( -15.45084971874737256, 49.38125000068280457, -47.55282581475767500 ) ) ;
#10150 = EDGE_CURVE ( 'NONE', #7907, #7744, #4784, .T. ) ;
#10151 = CARTESIAN_POINT ( 'NONE',  ( -15.45084971874737256, 23.60000000000000142, -47.55282581475767500 ) ) ;
#10152 = EDGE_CURVE ( 'NONE', #8881, #7781, #4948, .T. ) ;
#10153 = LINE ( 'NONE', #14965, #8671 ) ;
#10154 = ORIENTED_EDGE ( 'NONE', *, *, #2371, .F. ) ;
#10155 = CARTESIAN_POINT ( 'NONE',  ( 40.34137639590981905, 46.65937500034139873, 29.30972558990010768 ) ) ;
#10156 = ORIENTED_EDGE ( 'NONE', *, *, #14343, .F. ) ;
#10157 = CARTESIAN_POINT ( 'NONE',  ( 0.000000000000000000, 50.00000000000000000, -50.00000000000000000 ) ) ;
#10158 = VERTEX_POINT ( 'NONE', #8502 ) ;
#10159 = DIRECTION ( 'NONE',  ( -1.000000000000000000, 0.000000000000000000, 0.000000000000000000 ) ) ;
#10160 = CARTESIAN_POINT ( 'NONE',  ( 30.81806926056964002, 28.55937500034139731, 42.41743335407647209 ) ) ;
#10162 = EDGE_LOOP ( 'NONE', ( #5206, #15787, #13806, #1826, #12448, #7598, #4479, #14394, #7659, #24, #14784, #9261, #10816, #6653, #2316, #5535, #9488, #15500, #9795, #8716 ) ) ;
#10161 = AXIS2_PLACEMENT_3D ( 'NONE', #15376, #3999, #2738 ) ;
#10163 = CARTESIAN_POINT ( 'NONE',  ( 0.000000000000000000, 217.0000000000000284, 45.00000000000000000 ) ) ;
#10165 = EDGE_CURVE ( 'NONE', #13411, #15993, #9774, .T. ) ;
#10164 = FACE_OUTER_BOUND ( 'NONE', #9243, .T. ) ;
#10166 = CARTESIAN_POINT ( 'NONE',  ( 46.56218328577816123, 25.00000000000000000, -17.84593874833561955 ) ) ;
#10167 = CARTESIAN_POINT ( 'NONE',  ( 40.34137639590981195, 37.12187500034139731, -29.30972558990011834 ) ) ;
#10168 = DIRECTION ( 'NONE',  ( 0.000000000000000000, 0.000000000000000000, -1.000000000000000000 ) ) ;
#10169 = CARTESIAN_POINT ( 'NONE',  ( -49.86468353125000164, 25.85937500034139802, 0.000000000000000000 ) ) ;
#10170 = DIRECTION ( 'NONE',  ( -0.000000000000000000, -1.000000000000000000, -0.000000000000000000 ) ) ;
#10171 = CARTESIAN_POINT ( 'NONE',  ( -30.81806926056962226, 38.22187500034139873, 42.41743335407647209 ) ) ;
#10172 = DIRECTION ( 'NONE',  ( 0.000000000000000000, 0.000000000000000000, 1.000000000000000000 ) ) ;
#10173 = CARTESIAN_POINT ( 'NONE',  ( 50.00000000000000000, 31.00000000000000355, -6.123233995736766085E-15 ) ) ;
#10174 = CARTESIAN_POINT ( 'NONE',  ( -30.81806926056962226, 36.15937500034139163, 42.41743335407647919 ) ) ;
#10175 = CARTESIAN_POINT ( 'NONE',  ( -49.86468353125000164, 31.92187500034139447, 0.000000000000000000 ) ) ;
#10176 = VECTOR ( 'NONE', #14810, 1000.000000000000000 ) ;
#10177 = CARTESIAN_POINT ( 'NONE',  ( 15.45084971874737789, 44.60000000000000142, 47.55282581475767500 ) ) ;
#10178 = ORIENTED_EDGE ( 'NONE', *, *, #4990, .T. ) ;
#10179 = ORIENTED_EDGE ( 'NONE', *, *, #11373, .T. ) ;
#10180 = ADVANCED_FACE ( 'NONE', ( #1864 ), #6960, .T. ) ;
#10181 = CARTESIAN_POINT ( 'NONE',  ( 49.86468353124999453, 38.95937500034139589, -16.20201782572376104 ) ) ;
#10182 = ORIENTED_EDGE ( 'NONE', *, *, #2358, .F. ) ;
#10183 = ORIENTED_EDGE ( 'NONE', *, *, #4782, .F. ) ;
#10184 = CARTESIAN_POINT ( 'NONE',  ( 25.00000000000000355, 287.0000000000000568, -2.499999999999999556 ) ) ;
#10185 = CARTESIAN_POINT ( 'NONE',  ( 40.34137639590981195, 47.05937500034140442, -29.30972558990011834 ) ) ;
#10186 = DIRECTION ( 'NONE',  ( 0.000000000000000000, -0.000000000000000000, 1.000000000000000000 ) ) ;
#10187 = CARTESIAN_POINT ( 'NONE',  ( -15.40903463028481646, 25.52187500034139589, -47.42413220539093999 ) ) ;
#10188 = CIRCLE ( 'NONE', #3011, 5.000000000000000000 ) ;
#10189 = FACE_OUTER_BOUND ( 'NONE', #1291, .T. ) ;
#10190 = ADVANCED_FACE ( 'NONE', ( #8574 ), #2256, .T. ) ;
#10191 = CARTESIAN_POINT ( 'NONE',  ( -49.86468353124999453, 43.82187500034140015, -16.20201782572375393 ) ) ;
#10192 = LINE ( 'NONE', #12597, #697 ) ;
#10193 = CARTESIAN_POINT ( 'NONE',  ( 15.45084971874736723, 45.40000000000000568, -47.55282581475768211 ) ) ;
#10194 = EDGE_CURVE ( 'NONE', #12675, #2743, #5483, .T. ) ;
#10195 = CARTESIAN_POINT ( 'NONE',  ( -30.90169943749473802, 26.08125000068279320, 42.53254041760200721 ) ) ;
#10196 = CARTESIAN_POINT ( 'NONE',  ( -49.99999999999999289, 35.68125000068279462, -16.24598481164531449 ) ) ;
#10197 = CARTESIAN_POINT ( 'NONE',  ( -30.81806926056962226, 36.22187500034139873, 42.41743335407647919 ) ) ;
#10198 = CIRCLE ( 'NONE', #8064, 79.49773270518484480 ) ;
#10199 = CARTESIAN_POINT ( 'NONE',  ( -50.00000000000000000, 28.00000000000000000, 0.000000000000000000 ) ) ;
#10200 = VERTEX_POINT ( 'NONE', #14057 ) ;
#10201 = ORIENTED_EDGE ( 'NONE', *, *, #15079, .F. ) ;
#10202 = CARTESIAN_POINT ( 'NONE',  ( -7.919222016226934890, 32.44874571845316069, 49.99999999999996447 ) ) ;
#10203 = CARTESIAN_POINT ( 'NONE',  ( 0.5000000000000000000, 244.0000000000000284, -49.99999999999999289 ) ) ;
#10204 =( BOUNDED_CURVE ( )  B_SPLINE_CURVE ( 2, ( #13543, #14614, #1064, #14696, #14782, #8394, #7321, #2319, #9894, #3413, #12391, #12139, #13464 ),
 .UNSPECIFIED., .F., .F. ) 
 B_SPLINE_CURVE_WITH_KNOTS ( ( 3, 2, 2, 2, 2, 2, 3 ),
 ( 0.08333333333333334259, 0.08666666666666666963, 0.09333333333333333759, 0.1000000000000000056, 0.1066666666666666735, 0.1133333333333333276, 0.1166666666666666685 ),
 .UNSPECIFIED. ) 
 CURVE ( )  GEOMETRIC_REPRESENTATION_ITEM ( )  RATIONAL_B_SPLINE_CURVE ( ( 0.9755282581475768211, 0.9755282581475768211, 1.000000000000000000, 0.9510565162951535312, 1.000000000000000000, 0.9510565162951535312, 1.000000000000000000, 0.9510565162951535312, 1.000000000000000000, 0.9510565162951535312, 1.000000000000000000, 0.9755282581475767101, 0.9755282581475768211 ) ) 
 REPRESENTATION_ITEM ( '' )  );
#10205 = CARTESIAN_POINT ( 'NONE',  ( -15.45084971874737256, 23.60000000000000142, -47.55282581475767500 ) ) ;
#10206 = CARTESIAN_POINT ( 'NONE',  ( 0.000000000000000000, 257.0000000000001137, 0.000000000000000000 ) ) ;
#10207 = CARTESIAN_POINT ( 'NONE',  ( 9.631387414534489405E-15, 30.35937500034139447, 52.43083105670540789 ) ) ;
#10208 = EDGE_CURVE ( 'NONE', #15183, #6731, #6508, .T. ) ;
#10209 = VECTOR ( 'NONE', #15171, 1000.000000000000000 ) ;
#10210 = CARTESIAN_POINT ( 'NONE',  ( 9.631387414534489405E-15, 48.42187500034139447, 52.43083105670540789 ) ) ;
#10211 = CARTESIAN_POINT ( 'NONE',  ( -7.919222016226752814, 39.55125428154683931, -50.00000000000000711 ) ) ;
#10212 = CARTESIAN_POINT ( 'NONE',  ( -15.45084971874736368, 36.18125000068280173, 47.55282581475768211 ) ) ;
#10213 = CARTESIAN_POINT ( 'NONE',  ( 15.45084971874737789, 28.38125000068279746, 47.55282581475767500 ) ) ;
#10214 = ORIENTED_EDGE ( 'NONE', *, *, #251, .T. ) ;
#10215 = CARTESIAN_POINT ( 'NONE',  ( 30.81806926056962936, 49.22187500034139873, -42.41743335407647209 ) ) ;
#10216 = VERTEX_POINT ( 'NONE', #10243 ) ;
#10217 = CARTESIAN_POINT ( 'NONE',  ( -49.99999999999999289, 45.68125000068280173, -16.24598481164531449 ) ) ;
#10218 = EDGE_LOOP ( 'NONE', ( #15788, #5446, #15922, #3554 ) ) ;
#10219 = ORIENTED_EDGE ( 'NONE', *, *, #5489, .F. ) ;
#10220 = CIRCLE ( 'NONE', #11023, 17.50000000000000000 ) ;
#10221 = CARTESIAN_POINT ( 'NONE',  ( 0.000000000000000000, 193.4213562373095385, 0.000000000000000000 ) ) ;
#10222 = EDGE_CURVE ( 'NONE', #12433, #3981, #5279, .T. ) ;
#10223 = FACE_OUTER_BOUND ( 'NONE', #4086, .T. ) ;
#10224 = CARTESIAN_POINT ( 'NONE',  ( 0.000000000000000000, 20.00000000000000355, 50.00000000000000000 ) ) ;
#10225 = CARTESIAN_POINT ( 'NONE',  ( 0.000000000000000000, 20.00000000000000355, 0.000000000000000000 ) ) ;
#10226 = EDGE_CURVE ( 'NONE', #383, #9791, #8863, .T. ) ;
#10227 = CARTESIAN_POINT ( 'NONE',  ( 19.99999999999999645, 307.0000000000000568, 2.500000000000002220 ) ) ;
#10228 = CARTESIAN_POINT ( 'NONE',  ( 5.000000000000000000, 96.75198296766781425, 7.580410092413965017 ) ) ;
#10229 = DIRECTION ( 'NONE',  ( 0.000000000000000000, 0.000000000000000000, 1.000000000000000000 ) ) ;
#10230 = CYLINDRICAL_SURFACE ( 'NONE', #10728, 50.00000000000000000 ) ;
#10231 = CARTESIAN_POINT ( 'NONE',  ( -30.90169943749474868, 39.48125000068278467, -42.53254041760200721 ) ) ;
#10232 = CARTESIAN_POINT ( 'NONE',  ( 50.00000000000000711, 20.90000000000000213, 16.24598481164530739 ) ) ;
#10233 = CARTESIAN_POINT ( 'NONE',  ( 49.99999999999999289, 46.88125000068279036, -16.24598481164532160 ) ) ;
#10234 = ORIENTED_EDGE ( 'NONE', *, *, #2139, .T. ) ;
#10235 = CARTESIAN_POINT ( 'NONE',  ( 49.86468353125001585, 44.75937500034138594, 16.20201782572375038 ) ) ;
#10236 = VERTEX_POINT ( 'NONE', #2593 ) ;
#10237 = LINE ( 'NONE', #12808, #2519 ) ;
#10238 = CARTESIAN_POINT ( 'NONE',  ( -7.500000000000000000, 40.00000000000000711, -39.29058411375427795 ) ) ;
#10239 = CARTESIAN_POINT ( 'NONE',  ( 40.34137639590981195, 31.05937500034139731, -29.30972558990011834 ) ) ;
#10240 = VECTOR ( 'NONE', #11178, 1000.000000000000000 ) ;
#10241 = ORIENTED_EDGE ( 'NONE', *, *, #12818, .F. ) ;
#10242 = CARTESIAN_POINT ( 'NONE',  ( 40.45084971874737789, 26.80000000000000071, 29.38926261462365375 ) ) ;
#10243 = CARTESIAN_POINT ( 'NONE',  ( -2.547328955960238000E-13, 20.49999999999999645, 49.99999999999999289 ) ) ;
#10244 = VECTOR ( 'NONE', #3506, 1000.000000000000000 ) ;
#10245 = CARTESIAN_POINT ( 'NONE',  ( 46.68017951973684632, 24.99999999999999289, -17.53418100958397829 ) ) ;
#10246 = CARTESIAN_POINT ( 'NONE',  ( -15.40903463028481646, 35.52187500034139589, -47.42413220539093999 ) ) ;
#10247 = DIRECTION ( 'NONE',  ( -0.000000000000000000, 1.000000000000000000, -0.000000000000000000 ) ) ;
#10248 = CARTESIAN_POINT ( 'NONE',  ( -15.40903463028480580, 26.25937500034140015, 47.42413220539094709 ) ) ;
#10249 = CYLINDRICAL_SURFACE ( 'NONE', #7618, 50.00000000000000000 ) ;
#10250 = CARTESIAN_POINT ( 'NONE',  ( 30.81806926056962936, 29.22187500034139873, -42.41743335407646498 ) ) ;
#10251 = CARTESIAN_POINT ( 'NONE',  ( 0.000000000000000000, 20.00000000000000355, 0.000000000000000000 ) ) ;
#10252 = B_SPLINE_CURVE_WITH_KNOTS ( 'NONE', 3,
 ( #6940, #4358, #11992, #9511 ),
 .UNSPECIFIED., .F., .F.,
 ( 4, 4 ),
 ( 0.01002676606614814371, 0.01717959331248046853 ),
 .UNSPECIFIED. ) ;
#10253 = CARTESIAN_POINT ( 'NONE',  ( -15.45084971874736368, 30.40000000000000213, 47.55282581475768211 ) ) ;
#10254 = CARTESIAN_POINT ( 'NONE',  ( -40.34137639590981905, 35.65937500034139873, -29.30972558990011478 ) ) ;
#10255 = AXIS2_PLACEMENT_3D ( 'NONE', #7769, #195, #7611 ) ;
#10256 = CARTESIAN_POINT ( 'NONE',  ( 40.34137639590981195, 33.12187500034139731, -29.30972558990011834 ) ) ;
#10257 = TOROIDAL_SURFACE ( 'NONE', #15821, 63.16733765196516970, 2.000000000000000000 ) ;
#10258 = AXIS2_PLACEMENT_3D ( 'NONE', #10583, #653, #11732 ) ;
#10259 = CARTESIAN_POINT ( 'NONE',  ( 50.00000000000000711, 40.89999999999999858, 16.24598481164530739 ) ) ;
#10260 = ORIENTED_EDGE ( 'NONE', *, *, #1371, .T. ) ;
#10261 = AXIS2_PLACEMENT_3D ( 'NONE', #5566, #15511, #8033 ) ;
#10262 = UNCERTAINTY_MEASURE_WITH_UNIT (LENGTH_MEASURE( 1.000000000000000082E-05 ), #1216, 'distance_accuracy_value', 'NONE');
#10263 = CARTESIAN_POINT ( 'NONE',  ( -40.34137639590981195, 34.05937500034139731, 29.30972558990012189 ) ) ;
#10264 = EDGE_LOOP ( 'NONE', ( #4859, #7213, #11230, #8844, #6060, #7299, #4106, #16134, #3665, #10945, #11705, #12921, #4721, #15110, #13039, #11331, #12756, #10930, #6119, #11222, #15386, #939, #9302, #1742, #10837, #9564, #8974, #7067, #12069, #13414, #7099, #10815, #14055, #12753 ) ) ;
#10265 = ORIENTED_EDGE ( 'NONE', *, *, #6228, .T. ) ;
#10266 = CARTESIAN_POINT ( 'NONE',  ( 27.78424396843207234, 282.5058351977235134, -8.068487936863856902 ) ) ;
#10267 = CARTESIAN_POINT ( 'NONE',  ( 40.45084971874737079, 20.98125000068279888, -29.38926261462366440 ) ) ;
#10268 = AXIS2_PLACEMENT_3D ( 'NONE', #1266, #6357, #3852 ) ;
#10269 = PLANE ( 'NONE',  #1170 ) ;
#10270 = AXIS2_PLACEMENT_3D ( 'NONE', #10452, #12641, #13873 ) ;
#10271 = AXIS2_PLACEMENT_3D ( 'NONE', #4827, #14935, #11217 ) ;
#10272 = CARTESIAN_POINT ( 'NONE',  ( 49.86468353125001585, 20.82187500034140015, 16.20201782572375038 ) ) ;
#10273 = CIRCLE ( 'NONE', #5245, 40.00000000000000000 ) ;
#10274 = CARTESIAN_POINT ( 'NONE',  ( 8.446640517145639571E-15, 48.28125000068279604, 50.00000000000000000 ) ) ;
#10275 = CARTESIAN_POINT ( 'NONE',  ( -15.40903463028480580, 42.32187500034139305, 47.42413220539094709 ) ) ;
#10276 = CARTESIAN_POINT ( 'NONE',  ( -49.86468353125000164, 41.85937500034139447, 0.000000000000000000 ) ) ;
#10277 = CARTESIAN_POINT ( 'NONE',  ( 7.919222016226758143, 40.55125428154685352, 50.00000000000000711 ) ) ;
#10278 = EDGE_CURVE ( 'NONE', #9153, #15764, #13887, .T. ) ;
#10279 = CARTESIAN_POINT ( 'NONE',  ( 9.657523855033129090E-15, 44.50000000000000711, 52.57311121191334990 ) ) ;
#10280 = CARTESIAN_POINT ( 'NONE',  ( 40.45084971874737079, 26.98125000068279888, -29.38926261462366440 ) ) ;
#10281 = CARTESIAN_POINT ( 'NONE',  ( 17.39140362934560713, 24.75402226344611378, 94.04076213220706393 ) ) ;
#10282 = CARTESIAN_POINT ( 'NONE',  ( -15.40903463028481646, 31.52187500034139944, -47.42413220539093999 ) ) ;
#10284 = ADVANCED_FACE ( 'NONE', ( #15305 ), #7582, .F. ) ;
#10283 = CIRCLE ( 'NONE', #14494, 45.00000000000000000 ) ;
#10285 = ADVANCED_FACE ( 'NONE', ( #3844 ), #14136, .T. ) ;
#10286 = CARTESIAN_POINT ( 'NONE',  ( -3.111920190527341144E-15, 35.28125000068280315, -50.00000000000000000 ) ) ;
#10287 = ORIENTED_EDGE ( 'NONE', *, *, #14886, .F. ) ;
#10288 = CARTESIAN_POINT ( 'NONE',  ( 50.00000000000000000, 38.78125000068279604, -6.123233995736766085E-15 ) ) ;
#10289 = ORIENTED_EDGE ( 'NONE', *, *, #4782, .T. ) ;
#10290 = ADVANCED_FACE ( 'NONE', ( #10164 ), #7669, .F. ) ;
#10291 = PLANE ( 'NONE',  #10523 ) ;
#10292 = CARTESIAN_POINT ( 'NONE',  ( 7.919222016226809657, 45.44874571845314648, -50.00000000000000000 ) ) ;
#10293 = PLANE ( 'NONE',  #12094 ) ;
#10294 = CARTESIAN_POINT ( 'NONE',  ( -49.86468353124999453, 46.02187500034139589, 16.20201782572377169 ) ) ;
#10295 = CARTESIAN_POINT ( 'NONE',  ( -15.40903463028481646, 33.45937500034139589, -47.42413220539093999 ) ) ;
#10296 = CARTESIAN_POINT ( 'NONE',  ( -3.210462471511496205E-15, 49.42187500034138736, -52.43083105670540789 ) ) ;
#10297 = DIRECTION ( 'NONE',  ( 1.000000000000000000, 0.000000000000000000, 0.000000000000000000 ) ) ;
#10298 = DIRECTION ( 'NONE',  ( -0.000000000000000000, -1.000000000000000000, -0.000000000000000000 ) ) ;
#10299 = DIRECTION ( 'NONE',  ( -0.000000000000000000, 1.000000000000000000, -0.000000000000000000 ) ) ;
#10300 = CARTESIAN_POINT ( 'NONE',  ( 30.90169943749473802, 29.08125000068280031, -42.53254041760200721 ) ) ;
#10301 = ORIENTED_EDGE ( 'NONE', *, *, #11787, .F. ) ;
#10302 = CARTESIAN_POINT ( 'NONE',  ( -30.81806926056963292, 49.62187500034139020, -42.41743335407647209 ) ) ;
#10303 = ORIENTED_EDGE ( 'NONE', *, *, #5840, .T. ) ;
#10304 = CARTESIAN_POINT ( 'NONE',  ( -30.90169943749474513, 25.69999999999999574, -42.53254041760200721 ) ) ;
#10305 = VERTEX_POINT ( 'NONE', #174 ) ;
#10306 = ORIENTED_EDGE ( 'NONE', *, *, #832, .F. ) ;
#10307 =( BOUNDED_CURVE ( )  B_SPLINE_CURVE ( 2, ( #984, #7403, #14949, #2148, #6083, #10893, #12220, #11228, #4504, #9642, #822, #15957, #10971 ),
 .UNSPECIFIED., .F., .F. ) 
 B_SPLINE_CURVE_WITH_KNOTS ( ( 3, 2, 2, 2, 2, 2, 3 ),
 ( 0.3166666666666667074, 0.3200000000000000067, 0.3266666666666666607, 0.3333333333333333148, 0.3400000000000000244, 0.3466666666666666785, 0.3500000000000000333 ),
 .UNSPECIFIED. ) 
 CURVE ( )  GEOMETRIC_REPRESENTATION_ITEM ( )  RATIONAL_B_SPLINE_CURVE ( ( 0.9755282581475768211, 0.9755282581475770431, 1.000000000000000000, 0.9510565162951535312, 1.000000000000000000, 0.9510565162951535312, 1.000000000000000000, 0.9510565162951535312, 1.000000000000000000, 0.9510565162951535312, 1.000000000000000000, 0.9755282581475765991, 0.9755282581475768211 ) ) 
 REPRESENTATION_ITEM ( '' )  );
#10308 = CARTESIAN_POINT ( 'NONE',  ( 0.000000000000000000, 52.00000000000000711, 0.000000000000000000 ) ) ;
#10309 = LINE ( 'NONE', #14111, #3331 ) ;
#10310 = DIRECTION ( 'NONE',  ( 1.000000000000000000, 0.000000000000000000, 0.000000000000000000 ) ) ;
#10311 = FACE_OUTER_BOUND ( 'NONE', #2000, .T. ) ;
#10312 = CARTESIAN_POINT ( 'NONE',  ( -16.68146630878711534, 20.24395310072295828, 101.6666710451724214 ) ) ;
#10313 = DIRECTION ( 'NONE',  ( 0.9993309688977879413, -0.03657341386592747462, 0.000000000000000000 ) ) ;
#10314 = PLANE ( 'NONE',  #3811 ) ;
#10315 = DIRECTION ( 'NONE',  ( -0.9945218953682730678, -0.1045284632676570929, 0.000000000000000000 ) ) ;
#10316 = DIRECTION ( 'NONE',  ( 0.000000000000000000, 0.000000000000000000, 1.000000000000000000 ) ) ;
#10317 = CARTESIAN_POINT ( 'NONE',  ( 49.99999999999999289, 40.88125000068279036, -16.24598481164532160 ) ) ;
#10318 = CARTESIAN_POINT ( 'NONE',  ( -30.90169943749473802, 20.30000000000000426, 42.53254041760200721 ) ) ;
#10319 = CARTESIAN_POINT ( 'NONE',  ( -6.251299836021416922, 37.76994598419257443, 102.0000000000000142 ) ) ;
#10320 = VERTEX_POINT ( 'NONE', #7826 ) ;
#10321 = CARTESIAN_POINT ( 'NONE',  ( 9.631387414534489405E-15, 36.35937500034140157, 52.43083105670540789 ) ) ;
#10322 = ORIENTED_EDGE ( 'NONE', *, *, #11803, .T. ) ;
#10323 = DIRECTION ( 'NONE',  ( 0.000000000000000000, 1.000000000000000000, 0.000000000000000000 ) ) ;
#10324 = AXIS2_PLACEMENT_3D ( 'NONE', #3805, #11375, #16269 ) ;
#10325 = CARTESIAN_POINT ( 'NONE',  ( 7.513064459987437071E-14, 42.50000000000000000, 50.00000000000000000 ) ) ;
#10326 = CARTESIAN_POINT ( 'NONE',  ( 49.86468353125001585, 30.75937500034139305, 16.20201782572375038 ) ) ;
#10327 = ORIENTED_EDGE ( 'NONE', *, *, #14864, .T. ) ;
#10328 = ADVANCED_FACE ( 'NONE', ( #2751 ), #2925, .F. ) ;
#10329 = CYLINDRICAL_SURFACE ( 'NONE', #2554, 50.00000000000000000 ) ;
#10330 = CARTESIAN_POINT ( 'NONE',  ( -5.642626679385776889, 39.07526700153634636, 92.94045629140883591 ) ) ;
#10331 = CARTESIAN_POINT ( 'NONE',  ( 46.38089879718482678, 25.00000000000000000, -18.31192695794318226 ) ) ;
#10332 = CARTESIAN_POINT ( 'NONE',  ( 15.40903463028481113, 31.32187500034139305, -47.42413220539094709 ) ) ;
#10333 = CARTESIAN_POINT ( 'NONE',  ( -40.45084971874737079, 37.98125000068279888, 29.38926261462367151 ) ) ;
#10334 = CARTESIAN_POINT ( 'NONE',  ( 15.40903463028482356, 22.45937500034139589, 47.42413220539093999 ) ) ;
#10335 = FACE_OUTER_BOUND ( 'NONE', #11707, .T. ) ;
#10336 = CARTESIAN_POINT ( 'NONE',  ( -40.34137639590981195, 28.12187500034139731, 29.30972558990012189 ) ) ;
#10337 = CARTESIAN_POINT ( 'NONE',  ( -30.00000000000000711, 287.0000000000000568, 7.500000000000001776 ) ) ;
#10338 = CARTESIAN_POINT ( 'NONE',  ( -30.90169943749473802, 28.30000000000000071, 42.53254041760200721 ) ) ;
#10339 = CARTESIAN_POINT ( 'NONE',  ( -49.86468353124999453, 31.75937500034140015, -16.20201782572375393 ) ) ;
#10340 = CARTESIAN_POINT ( 'NONE',  ( -15.40903463028480580, 32.32187500034139305, 47.42413220539094709 ) ) ;
#10341 = ORIENTED_EDGE ( 'NONE', *, *, #14628, .T. ) ;
#10342 = CARTESIAN_POINT ( 'NONE',  ( 30.81806926056964002, 38.55937500034139731, 42.41743335407646498 ) ) ;
#10343 = ORIENTED_EDGE ( 'NONE', *, *, #15667, .F. ) ;
#10344 = EDGE_LOOP ( 'NONE', ( #5295, #4256, #6696, #16185, #14257 ) ) ;
#10345 = CARTESIAN_POINT ( 'NONE',  ( 25.07567824489208519, 285.0109613521088932, -7.575678244889592072 ) ) ;
#10346 = CARTESIAN_POINT ( 'NONE',  ( -3.210462471511496205E-15, 49.35937500034138736, -52.43083105670540789 ) ) ;
#10347 = VECTOR ( 'NONE', #4651, 1000.000000000000000 ) ;
#10348 = DIRECTION ( 'NONE',  ( 0.9781476007338069101, -0.2079116908177532641, 0.000000000000000000 ) ) ;
#10349 = CARTESIAN_POINT ( 'NONE',  ( -30.81806926056962226, 24.22187500034139163, 42.41743335407647919 ) ) ;
#10350 = DIRECTION ( 'NONE',  ( -5.069245582283711292E-17, -1.000000000000000000, 8.780190904559502465E-17 ) ) ;
#10351 = CARTESIAN_POINT ( 'NONE',  ( -40.34137639590981195, 36.12187500034139731, 29.30972558990012189 ) ) ;
#10352 = CARTESIAN_POINT ( 'NONE',  ( -40.34137639590981195, 42.05937500034139731, 29.30972558990012189 ) ) ;
#10353 = LINE ( 'NONE', #10112, #4448 ) ;
#10354 = CARTESIAN_POINT ( 'NONE',  ( -49.99999999999999289, 46.09999999999999432, 16.24598481164533226 ) ) ;
#10355 = CARTESIAN_POINT ( 'NONE',  ( 50.00000000000000000, 22.78125000068279959, -6.123233995736766085E-15 ) ) ;
#10356 = CARTESIAN_POINT ( 'NONE',  ( 49.86468353125000164, 48.92187500034139447, -6.106662507704105588E-15 ) ) ;
#10357 = EDGE_CURVE ( 'NONE', #11210, #7740, #8586, .T. ) ;
#10358 = STYLED_ITEM ( 'NONE', ( #3824 ), #3636 ) ;
#10359 = CARTESIAN_POINT ( 'NONE',  ( -40.34137639590981195, 26.12187500034139731, 29.30972558990012189 ) ) ;
#10360 = CARTESIAN_POINT ( 'NONE',  ( -7.919222016226804328, 28.22999571913594963, 50.00000000000000000 ) ) ;
#10361 = EDGE_LOOP ( 'NONE', ( #6840, #12216, #12468, #3281 ) ) ;
#10362 = CARTESIAN_POINT ( 'NONE',  ( -15.45084971874736368, 38.18125000068280173, 47.55282581475768211 ) ) ;
#10363 = ORIENTED_EDGE ( 'NONE', *, *, #10776, .F. ) ;
#10364 =( REPRESENTATION_RELATIONSHIP ('NONE','NONE', #6178, #5560 ) REPRESENTATION_RELATIONSHIP_WITH_TRANSFORMATION ( #13509 )SHAPE_REPRESENTATION_RELATIONSHIP( ) );
#10365 = LINE ( 'NONE', #10917, #15567 ) ;
#10366 = PLANE ( 'NONE',  #4406 ) ;
#10367 = CARTESIAN_POINT ( 'NONE',  ( 9.297345850538470396E-15, 92.00000000000001421, -1.969248798088869855E-14 ) ) ;
#10368 = CARTESIAN_POINT ( 'NONE',  ( 9.631387414534489405E-15, 46.42187500034139447, 52.43083105670540789 ) ) ;
#10369 =( BOUNDED_CURVE ( )  B_SPLINE_CURVE ( 2, ( #45, #4988, #11133, #9958, #3648, #2299, #13770, #13930, #1046, #7707, #4823, #8869, #5073 ),
 .UNSPECIFIED., .F., .F. ) 
 B_SPLINE_CURVE_WITH_KNOTS ( ( 3, 2, 2, 2, 2, 2, 3 ),
 ( 0.8500000000000000888, 0.8533333333333333881, 0.8599999999999999867, 0.8666666666666666963, 0.8733333333333332948, 0.8800000000000000044, 0.8833333333333334147 ),
 .UNSPECIFIED. ) 
 CURVE ( )  GEOMETRIC_REPRESENTATION_ITEM ( )  RATIONAL_B_SPLINE_CURVE ( ( 0.9755282581475768211, 0.9755282581475771542, 1.000000000000000000, 0.9510565162951535312, 1.000000000000000000, 0.9510565162951535312, 1.000000000000000000, 0.9510565162951535312, 1.000000000000000000, 0.9510565162951535312, 1.000000000000000000, 0.9755282581475763770, 0.9755282581475768211 ) ) 
 REPRESENTATION_ITEM ( '' )  );
#10370 = CARTESIAN_POINT ( 'NONE',  ( -49.86468353124999453, 25.95937500034139944, 16.20201782572377525 ) ) ;
#10371 = EDGE_CURVE ( 'NONE', #11171, #9838, #8381, .T. ) ;
#10372 = DIRECTION ( 'NONE',  ( 0.000000000000000000, 0.000000000000000000, 1.000000000000000000 ) ) ;
#10373 = FACE_OUTER_BOUND ( 'NONE', #6757, .T. ) ;
#10374 = CARTESIAN_POINT ( 'NONE',  ( 30.81806926056962936, 45.22187500034139873, -42.41743335407646498 ) ) ;
#10375 = PRODUCT_CONTEXT ( 'NONE', #12159, 'mechanical' ) ;
#10376 = FACE_OUTER_BOUND ( 'NONE', #5704, .T. ) ;
#10377 = B_SPLINE_CURVE_WITH_KNOTS ( 'NONE', 3,
 ( #5472, #15600, #13342, #1945 ),
 .UNSPECIFIED., .F., .F.,
 ( 4, 4 ),
 ( 2.829004760683457170E-07, 0.001414802801989366787 ),
 .UNSPECIFIED. ) ;
#10378 = CARTESIAN_POINT ( 'NONE',  ( -49.86468353125000164, 47.92187500034139447, 0.000000000000000000 ) ) ;
#10379 = ADVANCED_FACE ( 'NONE', ( #5754, #6851 ), #5433, .T. ) ;
#10380 = CARTESIAN_POINT ( 'NONE',  ( -3.111920190527341144E-15, 29.28125000068279604, -50.00000000000000000 ) ) ;
#10381 = ORIENTED_EDGE ( 'NONE', *, *, #6633, .T. ) ;
#10382 = CARTESIAN_POINT ( 'NONE',  ( -49.86468353124999453, 47.82187500034140015, -16.20201782572375393 ) ) ;
#10383 = VERTEX_POINT ( 'NONE', #15712 ) ;
#10384 = CARTESIAN_POINT ( 'NONE',  ( -3.111920190527341144E-15, 25.50000000000000355, -50.00000000000000000 ) ) ;
#10385 = VERTEX_POINT ( 'NONE', #573 ) ;
#10386 = EDGE_LOOP ( 'NONE', ( #9891, #818, #3578, #5385 ) ) ;
#10387 = EDGE_CURVE ( 'NONE', #58, #12729, #7992, .T. ) ;
#10388 = DIRECTION ( 'NONE',  ( 0.000000000000000000, 0.000000000000000000, 1.000000000000000000 ) ) ;
#10389 = DIRECTION ( 'NONE',  ( 1.000000000000000000, 0.000000000000000000, 0.000000000000000000 ) ) ;
#10390 = SURFACE_SIDE_STYLE ('',( #12792 ) ) ;
#10391 = CARTESIAN_POINT ( 'NONE',  ( -49.99999999999999289, 25.89999999999999858, -16.24598481164531449 ) ) ;
#10392 = CARTESIAN_POINT ( 'NONE',  ( 15.40903463028481113, 49.25937500034139305, -47.42413220539094709 ) ) ;
#10393 = CARTESIAN_POINT ( 'NONE',  ( 7.919222016226807881, 49.22999571913593542, -50.00000000000000000 ) ) ;
#10394 = CARTESIAN_POINT ( 'NONE',  ( 0.000000000000000000, 20.00000000000000355, 50.00000000000000000 ) ) ;
#10395 = CARTESIAN_POINT ( 'NONE',  ( -49.86468353124999453, 24.02187500034139589, 16.20201782572377525 ) ) ;
#10396 = CARTESIAN_POINT ( 'NONE',  ( 0.000000000000000000, 272.0000000000000000, 0.000000000000000000 ) ) ;
#10397 = CARTESIAN_POINT ( 'NONE',  ( -49.99999999999999289, 37.68125000068278752, -16.24598481164531449 ) ) ;
#10398 = CARTESIAN_POINT ( 'NONE',  ( -49.99999999999999289, 37.88125000068279746, 16.24598481164533226 ) ) ;
#10399 = EDGE_CURVE ( 'NONE', #16281, #11207, #5668, .T. ) ;
#10400 = CARTESIAN_POINT ( 'NONE',  ( -30.90169943749474868, 23.69999999999999929, -42.53254041760200721 ) ) ;
#10401 = FILL_AREA_STYLE_COLOUR ( '', #8138 ) ;
#10402 = ORIENTED_EDGE ( 'NONE', *, *, #10419, .F. ) ;
#10403 =( BOUNDED_CURVE ( )  B_SPLINE_CURVE ( 3, ( #12947, #11693, #4047, #10623 ),
 .UNSPECIFIED., .F., .T. ) 
 B_SPLINE_CURVE_WITH_KNOTS ( ( 4, 4 ),
 ( 2.558501865821650068, 3.141592653589793116 ),
 .UNSPECIFIED. ) 
 CURVE ( )  GEOMETRIC_REPRESENTATION_ITEM ( )  RATIONAL_B_SPLINE_CURVE ( ( 1.000000000000000000, 0.9718672150731670900, 0.9718672150731670900, 1.000000000000000000 ) ) 
 REPRESENTATION_ITEM ( '' )  );
#10404 = CARTESIAN_POINT ( 'NONE',  ( 9.631387414534489405E-15, 38.35937500034139447, 52.43083105670540789 ) ) ;
#10405 = VERTEX_POINT ( 'NONE', #10659 ) ;
#10406 = EDGE_CURVE ( 'NONE', #12541, #4002, #2874, .T. ) ;
#10407 = DIRECTION ( 'NONE',  ( 1.000000000000000000, 0.000000000000000000, 0.000000000000000000 ) ) ;
#10408 = DIRECTION ( 'NONE',  ( -0.000000000000000000, -1.000000000000000000, -0.000000000000000000 ) ) ;
#10409 = CARTESIAN_POINT ( 'NONE',  ( 49.86468353125000164, 30.85937500034139802, -6.106662507704105588E-15 ) ) ;
#10410 = ORIENTED_EDGE ( 'NONE', *, *, #15858, .T. ) ;
#10411 = CARTESIAN_POINT ( 'NONE',  ( 8.446640517145639571E-15, 26.50000000000000000, 50.00000000000000000 ) ) ;
#10412 = CARTESIAN_POINT ( 'NONE',  ( -16.48898053797772789, 28.38332565970911148, 101.0000000000000000 ) ) ;
#10413 = CARTESIAN_POINT ( 'NONE',  ( -15.40544456622763470, 14.18301270189214947, 101.0000000000000000 ) ) ;
#10414 = CARTESIAN_POINT ( 'NONE',  ( -49.86468353124999453, 33.82187500034138594, -16.20201782572375393 ) ) ;
#10415 = CARTESIAN_POINT ( 'NONE',  ( -49.99999999999999289, 29.88125000068279391, 16.24598481164533226 ) ) ;
#10416 = B_SPLINE_CURVE_WITH_KNOTS ( 'NONE', 3,
 ( #2663, #322, #4076, #10319 ),
 .UNSPECIFIED., .F., .F.,
 ( 4, 4 ),
 ( 2.829004760709176796E-07, 0.001414802801989367437 ),
 .UNSPECIFIED. ) ;
#10417 = FACE_OUTER_BOUND ( 'NONE', #15056, .T. ) ;
#10418 = CARTESIAN_POINT ( 'NONE',  ( -47.69912754770682284, 20.00000000000000355, 14.53642574140364019 ) ) ;
#10419 = EDGE_CURVE ( 'NONE', #11171, #6897, #3066, .T. ) ;
#10420 = CARTESIAN_POINT ( 'NONE',  ( 40.34137639590981905, 26.72187500034139518, 29.30972558990010768 ) ) ;
#10421 = CARTESIAN_POINT ( 'NONE',  ( 0.000000000000000000, 282.0000000000000000, 0.000000000000000000 ) ) ;
#10422 = CARTESIAN_POINT ( 'NONE',  ( -15.45084971874737256, 33.60000000000000142, -47.55282581475767500 ) ) ;
#10423 = CARTESIAN_POINT ( 'NONE',  ( -40.34137639590981905, 33.65937500034139873, -29.30972558990011478 ) ) ;
#10424 = CARTESIAN_POINT ( 'NONE',  ( -30.81806926056963292, 27.62187500034139731, -42.41743335407647209 ) ) ;
#10425 = CARTESIAN_POINT ( 'NONE',  ( -20.00000000000000711, 287.0000000000000568, -7.500000000000000888 ) ) ;
#10426 = ORIENTED_EDGE ( 'NONE', *, *, #1722, .T. ) ;
#10427 = CARTESIAN_POINT ( 'NONE',  ( -49.86468353124999453, 27.75937500034139660, -16.20201782572375393 ) ) ;
#10428 = VERTEX_POINT ( 'NONE', #14541 ) ;
#10429 = CARTESIAN_POINT ( 'NONE',  ( 27.49424662897629901, 282.6608420050619088, -7.488493257954151439 ) ) ;
#10430 = CARTESIAN_POINT ( 'NONE',  ( -40.34137639590981195, 46.05937500034139731, 29.30972558990012189 ) ) ;
#10431 = CARTESIAN_POINT ( 'NONE',  ( -49.99999999999999289, 38.10000000000000142, 16.24598481164533226 ) ) ;
#10432 = CARTESIAN_POINT ( 'NONE',  ( 30.00000000000000000, 282.0000000000000000, 12.50000000000000178 ) ) ;
#10433 = CARTESIAN_POINT ( 'NONE',  ( -7.499999999999987566, 40.00000000000000711, 2.602085213965205908E-15 ) ) ;
#10434 = CARTESIAN_POINT ( 'NONE',  ( 40.34137639590981195, 39.12187500034139731, -29.30972558990011834 ) ) ;
#10435 = CARTESIAN_POINT ( 'NONE',  ( -40.34137639590981905, 43.65937500034139163, -29.30972558990011478 ) ) ;
#10436 = CARTESIAN_POINT ( 'NONE',  ( -50.00000000000000000, 44.00000000000000711, 0.000000000000000000 ) ) ;
#10437 = CARTESIAN_POINT ( 'NONE',  ( 30.90169943749475578, 42.69999999999999574, 42.53254041760200010 ) ) ;
#10438 = AXIS2_PLACEMENT_3D ( 'NONE', #14185, #223, #15265 ) ;
#10439 = CARTESIAN_POINT ( 'NONE',  ( -30.90169943749473802, 20.08125000068279320, 42.53254041760200721 ) ) ;
#10440 = CARTESIAN_POINT ( 'NONE',  ( -15.40903463028480580, 48.32187500034140015, 47.42413220539094709 ) ) ;
#10441 = CARTESIAN_POINT ( 'NONE',  ( 15.40903463028482356, 30.52187500034139589, 47.42413220539093999 ) ) ;
#10442 = CARTESIAN_POINT ( 'NONE',  ( -7.919222016226804328, 28.44874571845315003, 50.00000000000000000 ) ) ;
#10443 = ORIENTED_EDGE ( 'NONE', *, *, #7269, .F. ) ;
#10444 = CARTESIAN_POINT ( 'NONE',  ( -15.45084971874737256, 37.38125000068279746, -47.55282581475767500 ) ) ;
#10445 = VECTOR ( 'NONE', #5606, 1000.000000000000000 ) ;
#10446 = ORIENTED_EDGE ( 'NONE', *, *, #12513, .F. ) ;
#10447 = CARTESIAN_POINT ( 'NONE',  ( -7.580410092413954359, 99.32916037694960210, 5.000000000000000000 ) ) ;
#10448 = LINE ( 'NONE', #1706, #10766 ) ;
#10449 = CARTESIAN_POINT ( 'NONE',  ( 49.99999999999999289, 32.88125000068280457, -16.24598481164532160 ) ) ;
#10450 = CARTESIAN_POINT ( 'NONE',  ( -49.86468353124999453, 45.82187500034140015, -16.20201782572375393 ) ) ;
#10451 = CARTESIAN_POINT ( 'NONE',  ( -30.81806926056962226, 22.15937500034139873, 42.41743335407647919 ) ) ;
#10452 = CARTESIAN_POINT ( 'NONE',  ( 0.000000000000000000, 193.4213562373095385, 0.000000000000000000 ) ) ;
#10453 = CARTESIAN_POINT ( 'NONE',  ( 49.86468353124999453, 39.02187500034138878, -16.20201782572376104 ) ) ;
#10454 = CARTESIAN_POINT ( 'NONE',  ( 0.000000000000000000, 0.000000000000000000, 0.000000000000000000 ) ) ;
#10455 = CARTESIAN_POINT ( 'NONE',  ( 49.40314992384931259, 25.00000000000000000, -8.200154929058095732 ) ) ;
#10456 = B_SPLINE_CURVE_WITH_KNOTS ( 'NONE', 3,
 ( #1123, #3647, #7463, #6304 ),
 .UNSPECIFIED., .F., .F.,
 ( 4, 4 ),
 ( 2.829004760671193191E-07, 0.001414802801989368305 ),
 .UNSPECIFIED. ) ;
#10457 = CARTESIAN_POINT ( 'NONE',  ( -15.40903463028480580, 48.32187500034140015, 47.42413220539094709 ) ) ;
#10458 = LINE ( 'NONE', #6395, #7774 ) ;
#10459 = ORIENTED_EDGE ( 'NONE', *, *, #6967, .F. ) ;
#10460 = CARTESIAN_POINT ( 'NONE',  ( 9.631387414534489405E-15, 46.42187500034139447, 52.43083105670540789 ) ) ;
#10461 = VERTEX_POINT ( 'NONE', #3169 ) ;
#10462 = CARTESIAN_POINT ( 'NONE',  ( -43.87482193696061472, 257.0000000000001137, -10.00000000000000178 ) ) ;
#10463 = ORIENTED_EDGE ( 'NONE', *, *, #11329, .T. ) ;
#10464 = ORIENTED_EDGE ( 'NONE', *, *, #2650, .T. ) ;
#10465 = CARTESIAN_POINT ( 'NONE',  ( 15.53071739328000334, 28.07196708982297295, 102.0000000000000142 ) ) ;
#10466 = CARTESIAN_POINT ( 'NONE',  ( 30.90169943749475223, 38.48125000068279888, 42.53254041760199300 ) ) ;
#10467 = CONICAL_SURFACE ( 'NONE', #6223, 49.99999999999999289, 0.7853981633974642662 ) ;
#10468 = CARTESIAN_POINT ( 'NONE',  ( 30.90169943749473802, 29.30000000000000071, -42.53254041760200721 ) ) ;
#10469 = CARTESIAN_POINT ( 'NONE',  ( -3.219174618344376363E-15, 27.50000000000000355, -52.57311121191334990 ) ) ;
#10470 = CARTESIAN_POINT ( 'NONE',  ( -30.81806926056962226, 42.15937500034139163, 42.41743335407647919 ) ) ;
#10471 = CARTESIAN_POINT ( 'NONE',  ( -40.45084971874737079, 25.98125000068279888, 29.38926261462367151 ) ) ;
#10472 = LINE ( 'NONE', #1813, #757 ) ;
#10473 = LINE ( 'NONE', #9390, #11595 ) ;
#10474 = PLANE ( 'NONE',  #13637 ) ;
#10475 = CARTESIAN_POINT ( 'NONE',  ( -15.45084971874736368, 40.18125000068280173, 47.55282581475768211 ) ) ;
#10476 = DIRECTION ( 'NONE',  ( 0.000000000000000000, 0.000000000000000000, 1.000000000000000000 ) ) ;
#10477 = EDGE_CURVE ( 'NONE', #6698, #7881, #7329, .T. ) ;
#10478 = LINE ( 'NONE', #8057, #5538 ) ;
#10479 = CARTESIAN_POINT ( 'NONE',  ( -7.500000000000000000, 40.00000000000000711, -39.29058411375427795 ) ) ;
#10480 = ORIENTED_EDGE ( 'NONE', *, *, #4528, .F. ) ;
#10481 = AXIS2_PLACEMENT_3D ( 'NONE', #193, #15487, #7931 ) ;
#10482 = CARTESIAN_POINT ( 'NONE',  ( -15.40903463028481646, 37.45937500034139589, -47.42413220539093999 ) ) ;
#10483 = EDGE_CURVE ( 'NONE', #10725, #5374, #9575, .T. ) ;
#10484 = ORIENTED_EDGE ( 'NONE', *, *, #15323, .T. ) ;
#10485 = ORIENTED_EDGE ( 'NONE', *, *, #12974, .F. ) ;
#10486 = EDGE_CURVE ( 'NONE', #13541, #12113, #13066, .T. ) ;
#10487 = CARTESIAN_POINT ( 'NONE',  ( -30.90169943749474868, 47.48125000068279178, -42.53254041760200721 ) ) ;
#10488 = PLANE ( 'NONE',  #2290 ) ;
#10489 = CARTESIAN_POINT ( 'NONE',  ( -30.81806926056962226, 20.15937500034139518, 42.41743335407647919 ) ) ;
#10490 = ORIENTED_EDGE ( 'NONE', *, *, #7836, .T. ) ;
#10491 = EDGE_CURVE ( 'NONE', #332, #12784, #9648, .T. ) ;
#10492 = B_SPLINE_CURVE_WITH_KNOTS ( 'NONE', 3,
 ( #4645, #15861, #9623, #13524 ),
 .UNSPECIFIED., .F., .F.,
 ( 4, 4 ),
 ( 2.829004760679149478E-07, 0.001414802801989366787 ),
 .UNSPECIFIED. ) ;
#10493 = DIRECTION ( 'NONE',  ( 0.000000000000000000, 1.000000000000000000, 0.000000000000000000 ) ) ;
#10494 = CARTESIAN_POINT ( 'NONE',  ( 15.45084971874737789, 22.60000000000000142, 47.55282581475767500 ) ) ;
#10495 = AXIS2_PLACEMENT_3D ( 'NONE', #1948, #3207, #15847 ) ;
#10496 = CARTESIAN_POINT ( 'NONE',  ( 0.000000000000000000, 22.50000000000000000, 101.0000000000000000 ) ) ;
#10497 = CARTESIAN_POINT ( 'NONE',  ( -30.81806926056962226, 26.22187500034139518, 42.41743335407647209 ) ) ;
#10498 = AXIS2_PLACEMENT_3D ( 'NONE', #15462, #9402, #9154 ) ;
#10499 = DIRECTION ( 'NONE',  ( -6.938893903907231459E-18, 1.000000000000000000, 5.551115123125782702E-17 ) ) ;
#10500 = CARTESIAN_POINT ( 'NONE',  ( 2.464234863135679188, 13.31155363843775064, 101.0000000000000000 ) ) ;
#10501 = CARTESIAN_POINT ( 'NONE',  ( -47.02241032844462154, 19.99999999999999645, 16.59456509147196357 ) ) ;
#10502 = CARTESIAN_POINT ( 'NONE',  ( -49.86468353125000164, 25.92187500034139802, 0.000000000000000000 ) ) ;
#10503 =( BOUNDED_SURFACE ( )  B_SPLINE_SURFACE ( 3, 2, ( 
 ( #6703, #13007, #443 ),
 ( #6944, #13248, #274 ),
 ( #1776, #7933, #521 ),
 ( #3021, #4114, #15662 ),
 ( #1610, #594, #9271 ),
 ( #11753, #15731, #11921 ),
 ( #12929, #8092, #354 ),
 ( #9515, #15581, #11676 ),
 ( #2776, #7849, #5616 ),
 ( #5454, #10519, #1532 ),
 ( #10757, #15817, #5378 ),
 ( #13166, #4362, #4451 ),
 ( #14474, #14327, #2944 ),
 ( #8011, #13085, #10605 ),
 ( #1691, #6788, #11832 ),
 ( #3109, #5544, #4284 ),
 ( #14398, #9348, #7268 ),
 ( #10842, #2012, #3268 ) ),
 .UNSPECIFIED., .F., .F., .T. ) 
 B_SPLINE_SURFACE_WITH_KNOTS ( ( 4, 2, 2, 2, 2, 2, 2, 2, 4 ),
 ( 3, 3 ),
 ( 1.570796326794896558, 1.767145867644258628, 1.963495408493620697, 2.159844949342982545, 2.356194490192344837, 2.552544031041707129, 2.748893571891068976, 2.945243112740430824, 3.141592653589793116 ),
 ( 0.000000000000000000, 1.000000000000000000 ),
 .UNSPECIFIED. ) 
 GEOMETRIC_REPRESENTATION_ITEM ( )  RATIONAL_B_SPLINE_SURFACE ( (
 ( 1.000000000000000000, 1.000000000000000000, 1.000000000000000000),
 ( 1.000000000000000000, 1.000000000000000000, 1.000000000000000000),
 ( 1.000000000000000000, 0.9967613244521498217, 1.000000000000000000),
 ( 1.000000000000000000, 0.9841171504955907867, 1.000000000000000000),
 ( 1.000000000000000000, 0.9747108043452232806, 1.000000000000000000),
 ( 1.000000000000000000, 0.9506740354170890583, 1.000000000000000000),
 ( 1.000000000000000000, 0.9360421842396996484, 1.000000000000000000),
 ( 1.000000000000000000, 0.9031650994466967619, 1.000000000000000000),
 ( 1.000000000000000000, 0.8849191470854951280, 1.000000000000000000),
 ( 1.000000000000000000, 0.8471316604833825092, 1.000000000000000000),
 ( 1.000000000000000000, 0.8275942695279743244, 1.000000000000000000),
 ( 1.000000000000000000, 0.7902180087153679588, 1.000000000000000000),
 ( 1.000000000000000000, 0.7723968217385259738, 1.000000000000000000),
 ( 1.000000000000000000, 0.7418334179586800747, 1.000000000000000000),
 ( 1.000000000000000000, 0.7291288939600593100, 1.000000000000000000),
 ( 1.000000000000000000, 0.7117460025832584858, 1.000000000000000000),
 ( 1.000000000000000000, 0.7070717283367141670, 1.000000000000000000),
 ( 1.000000000000000000, 0.7071067811865475727, 1.000000000000000000) ) ) 
 REPRESENTATION_ITEM ( '' )  SURFACE ( )  );
#10504 = CARTESIAN_POINT ( 'NONE',  ( -3.505380114644267575, 100.5662537783984334, -8.566253778398381868 ) ) ;
#10505 = CARTESIAN_POINT ( 'NONE',  ( -30.90169943749473802, 36.29999999999998295, 42.53254041760200721 ) ) ;
#10506 = CARTESIAN_POINT ( 'NONE',  ( 15.40903463028482356, 30.45937500034139589, 47.42413220539093999 ) ) ;
#10507 = CARTESIAN_POINT ( 'NONE',  ( 30.90169943749475223, 38.69999999999999574, 42.53254041760199300 ) ) ;
#10508 = ORIENTED_EDGE ( 'NONE', *, *, #13723, .F. ) ;
#10509 = AXIS2_PLACEMENT_3D ( 'NONE', #7887, #5492, #14517 ) ;
#10510 = CARTESIAN_POINT ( 'NONE',  ( -30.81806926056962226, 28.15937500034139518, 42.41743335407647209 ) ) ;
#10511 = ORIENTED_EDGE ( 'NONE', *, *, #1765, .F. ) ;
#10512 =( GEOMETRIC_REPRESENTATION_CONTEXT ( 3 ) GLOBAL_UNCERTAINTY_ASSIGNED_CONTEXT ( ( #14071 ) ) GLOBAL_UNIT_ASSIGNED_CONTEXT ( ( #10147, #6410, #11239 ) ) REPRESENTATION_CONTEXT ( 'NONE', 'WORKASPACE' ) );
#10513 = EDGE_CURVE ( 'NONE', #15703, #11171, #1070, .T. ) ;
#10514 = CARTESIAN_POINT ( 'NONE',  ( 0.000000000000000000, 193.4213562373095385, 0.000000000000000000 ) ) ;
#10515 = CARTESIAN_POINT ( 'NONE',  ( -15.40903463028481646, 43.45937500034139589, -47.42413220539093999 ) ) ;
#10516 = CARTESIAN_POINT ( 'NONE',  ( 2.500000000000000000, 242.0000000000000284, 47.99999999999999289 ) ) ;
#10517 = CARTESIAN_POINT ( 'NONE',  ( 25.15991675647091697, 285.7035871579553259, 2.819833512935955966 ) ) ;
#10518 = ADVANCED_FACE ( 'NONE', ( #4583 ), #15008, .T. ) ;
#10519 = CARTESIAN_POINT ( 'NONE',  ( -25.07567824489023778, 285.0109613520845073, 7.575678244889168411 ) ) ;
#10520 = CARTESIAN_POINT ( 'NONE',  ( 49.86468353124999453, 33.02187500034139589, -16.20201782572376459 ) ) ;
#10521 = CARTESIAN_POINT ( 'NONE',  ( 15.40903463028481113, 35.25937500034139305, -47.42413220539094709 ) ) ;
#10522 = AXIS2_PLACEMENT_3D ( 'NONE', #2977, #11954, #6976 ) ;
#10523 = AXIS2_PLACEMENT_3D ( 'NONE', #15097, #12608, #3724 ) ;
#10524 = CARTESIAN_POINT ( 'NONE',  ( 0.000000000000000000, 22.50000000000000000, 102.0000000000000142 ) ) ;
#10525 = AXIS2_PLACEMENT_3D ( 'NONE', #457, #4220, #536 ) ;
#10526 = CARTESIAN_POINT ( 'NONE',  ( -3.219174618344376363E-15, 39.49999999999999289, -52.57311121191334990 ) ) ;
#10527 = CARTESIAN_POINT ( 'NONE',  ( 9.657523855033129090E-15, 20.28125000068279959, 52.57311121191334990 ) ) ;
#10528 = CARTESIAN_POINT ( 'NONE',  ( -40.34137639590981905, 43.72187500034139873, -29.30972558990011478 ) ) ;
#10529 = COLOUR_RGB ( '', 0.66274510, 0.83137255, 0.94901961) ;
#10530 = CARTESIAN_POINT ( 'NONE',  ( 40.34137639590981905, 26.72187500034139518, 29.30972558990010768 ) ) ;
#10531 = CARTESIAN_POINT ( 'NONE',  ( 30.81806926056962936, 47.15937500034139163, -42.41743335407646498 ) ) ;
#10532 = ORIENTED_EDGE ( 'NONE', *, *, #3632, .F. ) ;
#10533 = VECTOR ( 'NONE', #2596, 1000.000000000000000 ) ;
#10534 = VECTOR ( 'NONE', #14893, 1000.000000000000227 ) ;
#10536 = CARTESIAN_POINT ( 'NONE',  ( -30.90169943749473802, 38.08125000068280031, 42.53254041760200721 ) ) ;
#10535 = CIRCLE ( 'NONE', #7610, 65.15972704814865324 ) ;
#10537 = EDGE_LOOP ( 'NONE', ( #11030, #7537, #8497, #10322 ) ) ;
#10538 = CARTESIAN_POINT ( 'NONE',  ( -2.547328955960238000E-13, 30.28125000068279604, 49.99999999999999289 ) ) ;
#10539 = LINE ( 'NONE', #6555, #7854 ) ;
#10540 = EDGE_CURVE ( 'NONE', #15183, #13963, #4521, .T. ) ;
#10541 = LINE ( 'NONE', #8028, #13691 ) ;
#10542 = CARTESIAN_POINT ( 'NONE',  ( -49.86468353125000164, 45.92187500034139447, 0.000000000000000000 ) ) ;
#10543 = EDGE_CURVE ( 'NONE', #8515, #7197, #16213, .T. ) ;
#10544 = CARTESIAN_POINT ( 'NONE',  ( -30.81806926056963292, 27.55937500034139376, -42.41743335407647209 ) ) ;
#10545 = PLANE ( 'NONE',  #9435 ) ;
#10546 = CARTESIAN_POINT ( 'NONE',  ( -49.86468353124999453, 40.02187500034139589, 16.20201782572377169 ) ) ;
#10547 = CIRCLE ( 'NONE', #10268, 17.50000000000000000 ) ;
#10548 = APPLICATION_PROTOCOL_DEFINITION ( 'draft international standard', 'automotive_design', 1998, #13844 ) ;
#10549 = CARTESIAN_POINT ( 'NONE',  ( 0.000000000000000000, 20.00000000000000355, 0.000000000000000000 ) ) ;
#10550 = CIRCLE ( 'NONE', #12668, 16.50000000000000711 ) ;
#10551 = CARTESIAN_POINT ( 'NONE',  ( 30.81806926056964002, 44.62187500034140442, 42.41743335407647209 ) ) ;
#10552 = CARTESIAN_POINT ( 'NONE',  ( 0.000000000000000000, 52.00000000000000711, 0.000000000000000000 ) ) ;
#10553 = ORIENTED_EDGE ( 'NONE', *, *, #4595, .T. ) ;
#10554 = CARTESIAN_POINT ( 'NONE',  ( 40.34137639590981905, 20.65937500034139873, 29.30972558990010768 ) ) ;
#10555 = ORIENTED_EDGE ( 'NONE', *, *, #12236, .T. ) ;
#10556 = CARTESIAN_POINT ( 'NONE',  ( -20.00000000000000355, 287.0000000000000568, 7.500000000000001776 ) ) ;
#10557 = ORIENTED_EDGE ( 'NONE', *, *, #4292, .T. ) ;
#10558 = AXIS2_PLACEMENT_3D ( 'NONE', #1911, #2161, #3510 ) ;
#10559 = DIRECTION ( 'NONE',  ( 0.7431448254773955764, -0.6691306063588567943, 0.000000000000000000 ) ) ;
#10560 = CARTESIAN_POINT ( 'NONE',  ( 0.000000000000000000, 193.4213562373095385, -50.00000000000000000 ) ) ;
#10561 = AXIS2_PLACEMENT_3D ( 'NONE', #6386, #11522, #10123 ) ;
#10562 = CARTESIAN_POINT ( 'NONE',  ( -45.00000000000000000, 262.0000000000000000, 10.00000000000000178 ) ) ;
#10563 = CARTESIAN_POINT ( 'NONE',  ( 50.00000000000000711, 22.90000000000000213, 16.24598481164530739 ) ) ;
#10564 = CARTESIAN_POINT ( 'NONE',  ( 49.86468353124999453, 44.95937500034139589, -16.20201782572376459 ) ) ;
#10565 = CARTESIAN_POINT ( 'NONE',  ( 8.446640517145639571E-15, 26.28125000068279959, 50.00000000000000000 ) ) ;
#10566 = DIRECTION ( 'NONE',  ( 0.000000000000000000, 1.000000000000000000, 0.000000000000000000 ) ) ;
#10567 = CARTESIAN_POINT ( 'NONE',  ( 0.000000000000000000, 22.50000000000000000, 101.0000000000000000 ) ) ;
#10568 = CARTESIAN_POINT ( 'NONE',  ( 7.499999999999998224, 40.00000000000000711, 24.29058411375428150 ) ) ;
#10569 = CARTESIAN_POINT ( 'NONE',  ( -49.99999999999999289, 39.68125000068280173, -16.24598481164531449 ) ) ;
#10570 = DIRECTION ( 'NONE',  ( -0.000000000000000000, -1.000000000000000000, -0.000000000000000000 ) ) ;
#10571 = CARTESIAN_POINT ( 'NONE',  ( 2.518620260143805467, 29.98137973985617677, -40.00000000000000711 ) ) ;
#10572 = CARTESIAN_POINT ( 'NONE',  ( -20.00000000000000355, 312.0000000000000568, 2.500000000000001332 ) ) ;
#10573 = ORIENTED_EDGE ( 'NONE', *, *, #6123, .F. ) ;
#10574 = CARTESIAN_POINT ( 'NONE',  ( 49.86468353124999453, 34.95937500034138878, -16.20201782572376459 ) ) ;
#10575 = ORIENTED_EDGE ( 'NONE', *, *, #12401, .F. ) ;
#10576 = VERTEX_POINT ( 'NONE', #16292 ) ;
#10577 = DIRECTION ( 'NONE',  ( 0.000000000000000000, 0.000000000000000000, 1.000000000000000000 ) ) ;
#10578 = CARTESIAN_POINT ( 'NONE',  ( 7.500000000000005329, 25.00000000000000355, -24.29058411375428506 ) ) ;
#10579 = CARTESIAN_POINT ( 'NONE',  ( -49.86468353124999453, 21.75937500034140015, -16.20201782572375393 ) ) ;
#10580 = VERTEX_POINT ( 'NONE', #8555 ) ;
#10581 = EDGE_CURVE ( 'NONE', #7494, #2831, #11463, .T. ) ;
#10582 = CARTESIAN_POINT ( 'NONE',  ( -0.1743114854953159432, 100.0076106038165165, 5.000000000000000000 ) ) ;
#10583 = CARTESIAN_POINT ( 'NONE',  ( 0.000000000000000000, 262.0000000000000000, 0.000000000000000000 ) ) ;
#10584 = CARTESIAN_POINT ( 'NONE',  ( 4.898587196589413026E-15, 32.49999999999999289, 40.00000000000000000 ) ) ;
#10585 = CARTESIAN_POINT ( 'NONE',  ( -30.81806926056962226, 30.22187500034139518, 42.41743335407647209 ) ) ;
#10586 = PLANE ( 'NONE',  #1487 ) ;
#10587 = CARTESIAN_POINT ( 'NONE',  ( 4.613455220948956104, 5.578608468406812904, 98.91547126341453122 ) ) ;
#10588 = CARTESIAN_POINT ( 'NONE',  ( -48.24365308685478482, 20.00000000000001066, 12.61207274729074790 ) ) ;
#10589 = CARTESIAN_POINT ( 'NONE',  ( -49.86468353124999453, 29.82187500034139660, -16.20201782572375393 ) ) ;
#10590 = EDGE_CURVE ( 'NONE', #14668, #12113, #8400, .T. ) ;
#10591 = CARTESIAN_POINT ( 'NONE',  ( -15.45084971874737256, 21.60000000000000142, -47.55282581475767500 ) ) ;
#10592 = CARTESIAN_POINT ( 'NONE',  ( -50.00000000000000000, 38.00000000000000711, 0.000000000000000000 ) ) ;
#10593 = CARTESIAN_POINT ( 'NONE',  ( -15.40903463028481646, 29.45937500034139589, -47.42413220539093999 ) ) ;
#10594 = DIRECTION ( 'NONE',  ( 0.000000000000000000, 0.000000000000000000, -1.000000000000000000 ) ) ;
#10595 = AXIS2_PLACEMENT_3D ( 'NONE', #8462, #1962, #13527 ) ;
#10596 = ADVANCED_FACE ( 'NONE', ( #4845 ), #8483, .T. ) ;
#10597 = VERTEX_POINT ( 'NONE', #12145 ) ;
#10598 = CARTESIAN_POINT ( 'NONE',  ( -40.34137639590981195, 28.05937500034139731, 29.30972558990012189 ) ) ;
#10599 = ORIENTED_EDGE ( 'NONE', *, *, #12600, .F. ) ;
#10600 = CARTESIAN_POINT ( 'NONE',  ( 6.123233995736766085E-15, 52.00000000000000711, 50.00000000000000000 ) ) ;
#10601 = CARTESIAN_POINT ( 'NONE',  ( -40.34137639590981195, 42.05937500034139731, 29.30972558990012189 ) ) ;
#10602 = ADVANCED_FACE ( 'NONE', ( #12226 ), #4928, .T. ) ;
#10603 = DIRECTION ( 'NONE',  ( -0.000000000000000000, 1.000000000000000000, -0.000000000000000000 ) ) ;
#10604 = FACE_OUTER_BOUND ( 'NONE', #11407, .T. ) ;
#10605 = CARTESIAN_POINT ( 'NONE',  ( -25.25536947722673986, 285.3889217077648368, 3.010738954466191331 ) ) ;
#10606 = CIRCLE ( 'NONE', #7148, 85.01963570546854498 ) ;
#10607 = CARTESIAN_POINT ( 'NONE',  ( -3.210462471511496205E-15, 37.42187500034140157, -52.43083105670540789 ) ) ;
#10608 = CARTESIAN_POINT ( 'NONE',  ( 40.34137639590981195, 35.05937500034139731, -29.30972558990011834 ) ) ;
#10609 = LINE ( 'NONE', #15822, #16351 ) ;
#10610 = CARTESIAN_POINT ( 'NONE',  ( 40.45084971874737789, 40.80000000000000426, 29.38926261462365375 ) ) ;
#10611 = CARTESIAN_POINT ( 'NONE',  ( -49.99999999999999289, 21.88125000068280102, 16.24598481164533226 ) ) ;
#10612 = CARTESIAN_POINT ( 'NONE',  ( -15.40903463028480580, 42.32187500034139305, 47.42413220539094709 ) ) ;
#10613 = CARTESIAN_POINT ( 'NONE',  ( 40.34137639590981195, 27.12187500034139731, -29.30972558990011834 ) ) ;
#10614 = VECTOR ( 'NONE', #16441, 1000.000000000000000 ) ;
#10615 = DIRECTION ( 'NONE',  ( 0.000000000000000000, 0.000000000000000000, -1.000000000000000000 ) ) ;
#10616 = VERTEX_POINT ( 'NONE', #12303 ) ;
#10618 = EDGE_CURVE ( 'NONE', #6571, #8515, #7083, .T. ) ;
#10617 = CARTESIAN_POINT ( 'NONE',  ( 30.90169943749474157, 29.08125000068280031, -42.53254041760200721 ) ) ;
#10619 = VERTEX_POINT ( 'NONE', #904 ) ;
#10620 = CARTESIAN_POINT ( 'NONE',  ( 0.000000000000000000, 247.0000000000000284, 0.000000000000000000 ) ) ;
#10621 = CARTESIAN_POINT ( 'NONE',  ( -17.50000000000000000, 22.50000000000000000, 94.42467108177066848 ) ) ;
#10622 = CARTESIAN_POINT ( 'NONE',  ( -49.99999999999999289, 33.68125000068278752, -16.24598481164531449 ) ) ;
#10623 = CARTESIAN_POINT ( 'NONE',  ( 9.234334497652928468E-15, 101.0808929720139702, -9.080892972013931086 ) ) ;
#10624 = CARTESIAN_POINT ( 'NONE',  ( 40.34137639590981195, 27.05937500034139731, -29.30972558990011834 ) ) ;
#10625 = DIRECTION ( 'NONE',  ( -0.000000000000000000, -1.000000000000000000, -0.000000000000000000 ) ) ;
#10626 = CARTESIAN_POINT ( 'NONE',  ( 30.81806926056962936, 41.22187500034139873, -42.41743335407646498 ) ) ;
#10627 = CIRCLE ( 'NONE', #5589, 63.16733765196516970 ) ;
#10628 = CARTESIAN_POINT ( 'NONE',  ( 0.000000000000000000, 0.000000000000000000, 0.000000000000000000 ) ) ;
#10629 = CARTESIAN_POINT ( 'NONE',  ( -30.81806926056962226, 48.22187500034139163, 42.41743335407647919 ) ) ;
#10630 = DIRECTION ( 'NONE',  ( 0.000000000000000000, 0.000000000000000000, -1.000000000000000000 ) ) ;
#10631 = EDGE_LOOP ( 'NONE', ( #6446, #4215, #14206, #6798 ) ) ;
#10632 = CARTESIAN_POINT ( 'NONE',  ( -49.86468353124999453, 41.82187500034140015, -16.20201782572375393 ) ) ;
#10633 = EDGE_CURVE ( 'NONE', #2524, #14905, #1203, .T. ) ;
#10634 = ORIENTED_EDGE ( 'NONE', *, *, #11535, .F. ) ;
#10635 = ORIENTED_EDGE ( 'NONE', *, *, #9772, .F. ) ;
#10636 = CARTESIAN_POINT ( 'NONE',  ( 0.000000000000000000, 25.00000000000000355, 0.000000000000000000 ) ) ;
#10637 = DIRECTION ( 'NONE',  ( 0.000000000000000000, 0.000000000000000000, -1.000000000000000000 ) ) ;
#10638 = CARTESIAN_POINT ( 'NONE',  ( 6.123233995736766085E-15, 20.00000000000000355, -50.00000000000000000 ) ) ;
#10639 = CARTESIAN_POINT ( 'NONE',  ( 30.90169943749474157, 27.29999999999999716, -42.53254041760200721 ) ) ;
#10640 = CARTESIAN_POINT ( 'NONE',  ( 40.34137639590981195, 47.05937500034140442, -29.30972558990011834 ) ) ;
#10641 = CARTESIAN_POINT ( 'NONE',  ( 50.00000000000000711, 48.68125000068279462, 16.24598481164530739 ) ) ;
#10642 = LINE ( 'NONE', #393, #10865 ) ;
#10643 = CARTESIAN_POINT ( 'NONE',  ( -40.45084971874737079, 46.20000000000000284, 29.38926261462367151 ) ) ;
#10644 = CARTESIAN_POINT ( 'NONE',  ( 7.919222016226822092, 48.55125428154684641, 49.99999999999999289 ) ) ;
#10645 = CARTESIAN_POINT ( 'NONE',  ( -3.219174618344376363E-15, 37.28125000068280315, -52.57311121191334990 ) ) ;
#10646 =( BOUNDED_CURVE ( )  B_SPLINE_CURVE ( 2, ( #10380, #15356, #11532, #10300, #7877, #5398, #13033, #3976, #9125, #7796, #10213, #9299, #2894 ),
 .UNSPECIFIED., .F., .F. ) 
 B_SPLINE_CURVE_WITH_KNOTS ( ( 3, 2, 2, 2, 2, 2, 3 ),
 ( 0.6833333333333333481, 0.6866666666666666474, 0.6933333333333333570, 0.6999999999999999556, 0.7066666666666666652, 0.7133333333333333748, 0.7166666666666666741 ),
 .UNSPECIFIED. ) 
 CURVE ( )  GEOMETRIC_REPRESENTATION_ITEM ( )  RATIONAL_B_SPLINE_CURVE ( ( 0.9755282581475768211, 0.9755282581475768211, 1.000000000000000000, 0.9510565162951535312, 1.000000000000000000, 0.9510565162951535312, 1.000000000000000000, 0.9510565162951535312, 1.000000000000000000, 0.9510565162951535312, 1.000000000000000000, 0.9755282581475768211, 0.9755282581475768211 ) ) 
 REPRESENTATION_ITEM ( '' )  );
#10647 = CARTESIAN_POINT ( 'NONE',  ( 0.000000000000000000, 272.0000000000000000, 0.000000000000000000 ) ) ;
#10648 = CARTESIAN_POINT ( 'NONE',  ( -49.72257916183962578, 96.64601816452537264, -5.000000000000000000 ) ) ;
#10649 = CARTESIAN_POINT ( 'NONE',  ( 7.499999999999994671, 40.00000000000000711, 24.29058411375428150 ) ) ;
#10650 = ORIENTED_EDGE ( 'NONE', *, *, #7766, .T. ) ;
#10651 = CARTESIAN_POINT ( 'NONE',  ( 30.81806926056964002, 40.55937500034139731, 42.41743335407647209 ) ) ;
#10652 = ORIENTED_EDGE ( 'NONE', *, *, #41, .T. ) ;
#10653 = EDGE_LOOP ( 'NONE', ( #8197, #7479 ) ) ;
#10654 = CARTESIAN_POINT ( 'NONE',  ( -49.99999999999999289, 47.68125000068280173, -16.24598481164531449 ) ) ;
#10655 = DIRECTION ( 'NONE',  ( -0.000000000000000000, -1.000000000000000000, -0.000000000000000000 ) ) ;
#10656 = CARTESIAN_POINT ( 'NONE',  ( 9.631387414534489405E-15, 24.35937500034139802, 52.43083105670540789 ) ) ;
#10657 = ORIENTED_EDGE ( 'NONE', *, *, #15660, .F. ) ;
#10658 = CARTESIAN_POINT ( 'NONE',  ( -15.45084971874737256, 47.60000000000000142, -47.55282581475767500 ) ) ;
#10659 = CARTESIAN_POINT ( 'NONE',  ( 3.407225380398686276, 31.38205016914263723, 101.0000000000000000 ) ) ;
#10660 = DIRECTION ( 'NONE',  ( 0.3420201433256698231, 0.6644630243886754384, -0.6644630243886734400 ) ) ;
#10661 = CARTESIAN_POINT ( 'NONE',  ( 30.81806926056962936, 25.22187500034139873, -42.41743335407646498 ) ) ;
#10662 = ADVANCED_FACE ( 'NONE', ( #13549 ), #10899, .F. ) ;
#10663 = LINE ( 'NONE', #15471, #3624 ) ;
#10664 = EDGE_CURVE ( 'NONE', #10059, #12675, #2280, .T. ) ;
#10665 = LINE ( 'NONE', #8243, #2481 ) ;
#10666 = CARTESIAN_POINT ( 'NONE',  ( -47.29342682910125717, 19.99999999999999645, 15.80652463092984839 ) ) ;
#10667 = CARTESIAN_POINT ( 'NONE',  ( -15.40903463028480580, 22.32187500034139660, 47.42413220539094709 ) ) ;
#10668 = CARTESIAN_POINT ( 'NONE',  ( -2.499999999999999556, 247.0000000000000568, -49.17157287525380127 ) ) ;
#10669 = CARTESIAN_POINT ( 'NONE',  ( 40.45084971874737079, 37.20000000000000284, -29.38926261462366440 ) ) ;
#10670 = CARTESIAN_POINT ( 'NONE',  ( -15.40903463028481646, 33.45937500034139589, -47.42413220539093999 ) ) ;
#10671 = LINE ( 'NONE', #9260, #2733 ) ;
#10672 = EDGE_LOOP ( 'NONE', ( #10219, #9130, #548, #11653, #11869 ) ) ;
#10673 = CARTESIAN_POINT ( 'NONE',  ( 9.631387414534489405E-15, 30.35937500034139092, 52.43083105670540789 ) ) ;
#10674 = ORIENTED_EDGE ( 'NONE', *, *, #2724, .T. ) ;
#10675 = EDGE_CURVE ( 'NONE', #532, #14319, #5918, .T. ) ;
#10676 = DIRECTION ( 'NONE',  ( -1.000000000000000000, 0.000000000000000000, -0.000000000000000000 ) ) ;
#10677 = CARTESIAN_POINT ( 'NONE',  ( 49.86468353125000164, 44.85937500034140157, -6.106662507704105588E-15 ) ) ;
#10678 = CARTESIAN_POINT ( 'NONE',  ( 25.66084200510923807, 284.4942466289053868, 3.821684010227777595 ) ) ;
#10679 = PLANE ( 'NONE',  #11594 ) ;
#10680 = CARTESIAN_POINT ( 'NONE',  ( -30.81806926056962226, 36.22187500034139873, 42.41743335407647919 ) ) ;
#10681 = CARTESIAN_POINT ( 'NONE',  ( 40.34137639590981195, 37.05937500034139731, -29.30972558990011834 ) ) ;
#10682 = CARTESIAN_POINT ( 'NONE',  ( -49.99999999999999289, 43.89999999999999858, -16.24598481164531449 ) ) ;
#10683 = CARTESIAN_POINT ( 'NONE',  ( -30.90169943749474868, 39.70000000000000284, -42.53254041760200721 ) ) ;
#10684 = CARTESIAN_POINT ( 'NONE',  ( -40.45084971874737079, 23.98125000068279888, 29.38926261462367151 ) ) ;
#10685 = CARTESIAN_POINT ( 'NONE',  ( -15.40903463028481646, 41.52187500034139589, -47.42413220539093999 ) ) ;
#10686 = ADVANCED_FACE ( 'NONE', ( #4765 ), #4670, .F. ) ;
#10687 = CARTESIAN_POINT ( 'NONE',  ( 30.81806926056964002, 30.62187500034139020, 42.41743335407647209 ) ) ;
#10688 = CARTESIAN_POINT ( 'NONE',  ( 49.86468353125001585, 46.75937500034140015, 16.20201782572375038 ) ) ;
#10689 = VERTEX_POINT ( 'NONE', #14873 ) ;
#10690 = CARTESIAN_POINT ( 'NONE',  ( 30.90169943749475578, 28.48125000068280244, 42.53254041760200010 ) ) ;
#10691 = EDGE_LOOP ( 'NONE', ( #8479, #3735, #302, #4625 ) ) ;
#10692 = CYLINDRICAL_SURFACE ( 'NONE', #5218, 50.00000000000000000 ) ;
#10693 = VECTOR ( 'NONE', #7714, 1000.000000000000000 ) ;
#10694 = EDGE_CURVE ( 'NONE', #9644, #16281, #3502, .T. ) ;
#10695 = CARTESIAN_POINT ( 'NONE',  ( -30.90169943749473447, 34.08125000068279320, 42.53254041760200721 ) ) ;
#10696 = CARTESIAN_POINT ( 'NONE',  ( -3.210462471511496205E-15, 41.42187500034139447, -52.43083105670540789 ) ) ;
#10697 = CARTESIAN_POINT ( 'NONE',  ( 49.86468353124999453, 26.95937500034139944, -16.20201782572376459 ) ) ;
#10698 = CARTESIAN_POINT ( 'NONE',  ( 0.000000000000000000, 22.50000000000000000, 102.0000000000000142 ) ) ;
#10699 = CARTESIAN_POINT ( 'NONE',  ( 50.00000000000000000, 35.00000000000000000, -6.123233995736766085E-15 ) ) ;
#10700 = CARTESIAN_POINT ( 'NONE',  ( -49.86468353124999453, 44.02187500034139589, 16.20201782572377525 ) ) ;
#10701 = DIRECTION ( 'NONE',  ( 0.000000000000000000, 0.000000000000000000, 1.000000000000000000 ) ) ;
#10702 = VERTEX_POINT ( 'NONE', #7483 ) ;
#10703 = VECTOR ( 'NONE', #14885, 1000.000000000000000 ) ;
#10704 = CARTESIAN_POINT ( 'NONE',  ( -49.86468353124999453, 43.82187500034140015, -16.20201782572375393 ) ) ;
#10705 = VERTEX_POINT ( 'NONE', #2730 ) ;
#10706 = ORIENTED_EDGE ( 'NONE', *, *, #112, .F. ) ;
#10707 = EDGE_CURVE ( 'NONE', #13593, #5951, #12375, .T. ) ;
#10708 = DIRECTION ( 'NONE',  ( 0.000000000000000000, 0.000000000000000000, 1.000000000000000000 ) ) ;
#10709 = CARTESIAN_POINT ( 'NONE',  ( 0.000000000000000000, 20.00000000000000355, 50.00000000000000000 ) ) ;
#10710 = EDGE_CURVE ( 'NONE', #7385, #14428, #12916, .T. ) ;
#10711 = CYLINDRICAL_SURFACE ( 'NONE', #16195, 50.00000000000000000 ) ;
#10712 = CARTESIAN_POINT ( 'NONE',  ( -15.45084971874736368, 22.39999999999999858, 47.55282581475768211 ) ) ;
#10713 = CARTESIAN_POINT ( 'NONE',  ( 49.86468353125001585, 44.75937500034138594, 16.20201782572375038 ) ) ;
#10714 = CARTESIAN_POINT ( 'NONE',  ( -15.40903463028481646, 49.45937500034140299, -47.42413220539093999 ) ) ;
#10715 = DIRECTION ( 'NONE',  ( 0.000000000000000000, 0.000000000000000000, -1.000000000000000000 ) ) ;
#10716 = CARTESIAN_POINT ( 'NONE',  ( -49.99999999999999289, 33.88125000068280457, 16.24598481164533226 ) ) ;
#10717 = SURFACE_STYLE_FILL_AREA ( #2825 ) ;
#10718 = FACE_OUTER_BOUND ( 'NONE', #13337, .T. ) ;
#10719 = CARTESIAN_POINT ( 'NONE',  ( -7.919222016226816763, 45.55125428154684641, -49.99999999999999289 ) ) ;
#10720 = CARTESIAN_POINT ( 'NONE',  ( 50.00000000000000711, 46.68125000068279462, 16.24598481164530739 ) ) ;
#10721 = CARTESIAN_POINT ( 'NONE',  ( 21.39877161664097471, 15.54711762656373786, 101.0000000000000000 ) ) ;
#10722 = ORIENTED_EDGE ( 'NONE', *, *, #6886, .F. ) ;
#10723 = CARTESIAN_POINT ( 'NONE',  ( 30.81806926056962936, 33.15937500034139873, -42.41743335407647209 ) ) ;
#10724 = ORIENTED_EDGE ( 'NONE', *, *, #14051, .T. ) ;
#10725 = VERTEX_POINT ( 'NONE', #11545 ) ;
#10726 = ORIENTED_EDGE ( 'NONE', *, *, #15048, .F. ) ;
#10727 = EDGE_CURVE ( 'NONE', #15172, #2810, #684, .T. ) ;
#10728 = AXIS2_PLACEMENT_3D ( 'NONE', #12724, #8983, #11318 ) ;
#10729 = CARTESIAN_POINT ( 'NONE',  ( -3.219174618344376363E-15, 49.28125000068278894, -52.57311121191334990 ) ) ;
#10730 = EDGE_CURVE ( 'NONE', #2646, #7238, #14219, .T. ) ;
#10731 = LINE ( 'NONE', #4418, #8674 ) ;
#10732 = CARTESIAN_POINT ( 'NONE',  ( -30.81806926056963292, 23.55937500034139376, -42.41743335407647209 ) ) ;
#10733 = ORIENTED_EDGE ( 'NONE', *, *, #2952, .T. ) ;
#10734 = DIRECTION ( 'NONE',  ( 0.000000000000000000, 0.000000000000000000, -1.000000000000000000 ) ) ;
#10735 = CARTESIAN_POINT ( 'NONE',  ( -48.69930661242911185, 95.73172307475269349, -7.581784256837400982 ) ) ;
#10736 = LINE ( 'NONE', #4427, #14666 ) ;
#10737 = CARTESIAN_POINT ( 'NONE',  ( -40.34137639590981195, 28.12187500034139731, 29.30972558990012189 ) ) ;
#10738 =( BOUNDED_CURVE ( )  B_SPLINE_CURVE ( 2, ( #4581, #4204, #9645, #4111, #5542, #10431, #10896, #6701, #12926, #4282, #9267, #9181, #745 ),
 .UNSPECIFIED., .F., .F. ) 
 B_SPLINE_CURVE_WITH_KNOTS ( ( 3, 2, 2, 2, 2, 2, 3 ),
 ( 0.3833333333333333592, 0.3866666666666666585, 0.3933333333333333126, 0.4000000000000000222, 0.4066666666666666763, 0.4133333333333333304, 0.4166666666666666852 ),
 .UNSPECIFIED. ) 
 CURVE ( )  GEOMETRIC_REPRESENTATION_ITEM ( )  RATIONAL_B_SPLINE_CURVE ( ( 0.9755282581475768211, 0.9755282581475770431, 1.000000000000000000, 0.9510565162951535312, 1.000000000000000000, 0.9510565162951535312, 1.000000000000000000, 0.9510565162951535312, 1.000000000000000000, 0.9510565162951535312, 1.000000000000000000, 0.9755282581475765991, 0.9755282581475768211 ) ) 
 REPRESENTATION_ITEM ( '' )  );
#10739 = EDGE_CURVE ( 'NONE', #8437, #9035, #3990, .T. ) ;
#10740 = CARTESIAN_POINT ( 'NONE',  ( 0.000000000000000000, 22.50000000000000000, 102.0000000000000142 ) ) ;
#10741 = CARTESIAN_POINT ( 'NONE',  ( 15.96528350601207613, 15.31079395116513986, 95.98183428236838211 ) ) ;
#10742 = DIRECTION ( 'NONE',  ( -0.000000000000000000, 1.000000000000000000, -0.000000000000000000 ) ) ;
#10743 = CARTESIAN_POINT ( 'NONE',  ( 30.81806926056964002, 20.62187500034139020, 42.41743335407646498 ) ) ;
#10744 = CARTESIAN_POINT ( 'NONE',  ( -40.45084971874737789, 21.80000000000000071, -29.38926261462365730 ) ) ;
#10745 = AXIS2_PLACEMENT_3D ( 'NONE', #6728, #5478, #11774 ) ;
#10746 = CARTESIAN_POINT ( 'NONE',  ( -3.219174618344376363E-15, 35.50000000000000000, -52.57311121191334990 ) ) ;
#10747 = CARTESIAN_POINT ( 'NONE',  ( -30.81806926056962226, 24.15937500034139873, 42.41743335407647919 ) ) ;
#10748 = CARTESIAN_POINT ( 'NONE',  ( -49.86468353124999453, 47.75937500034139305, -16.20201782572375393 ) ) ;
#10749 = ORIENTED_EDGE ( 'NONE', *, *, #7880, .F. ) ;
#10750 = CARTESIAN_POINT ( 'NONE',  ( -49.86468353125000164, 31.85937500034139447, 0.000000000000000000 ) ) ;
#10751 = VERTEX_POINT ( 'NONE', #12720 ) ;
#10752 = FACE_BOUND ( 'NONE', #16305, .T. ) ;
#10753 = CARTESIAN_POINT ( 'NONE',  ( 49.86468353124999453, 44.95937500034139589, -16.20201782572376459 ) ) ;
#10754 = PRESENTATION_LAYER_ASSIGNMENT (  '', '', ( #15256 ) ) ;
#10755 = B_SPLINE_CURVE_WITH_KNOTS ( 'NONE', 3,
 ( #15429, #4049, #14959, #3747 ),
 .UNSPECIFIED., .F., .F.,
 ( 4, 4 ),
 ( 0.01140363079879802566, 0.01281815069648909247 ),
 .UNSPECIFIED. ) ;
#10756 = CARTESIAN_POINT ( 'NONE',  ( 24.93825083352558636, 285.3724546740382948, 7.438250833535430928 ) ) ;
#10757 = CARTESIAN_POINT ( 'NONE',  ( -22.04892374372078834, 283.9500510409134790, 8.524461871855393724 ) ) ;
#10758 = CARTESIAN_POINT ( 'NONE',  ( -30.81806926056962226, 28.22187500034139873, 42.41743335407647919 ) ) ;
#10759 = CARTESIAN_POINT ( 'NONE',  ( 15.40903463028482356, 34.45937500034139589, 47.42413220539093999 ) ) ;
#10760 = CARTESIAN_POINT ( 'NONE',  ( -2.547328955960238000E-13, 32.50000000000000000, 49.99999999999999289 ) ) ;
#10761 = CARTESIAN_POINT ( 'NONE',  ( -49.86468353125000164, 29.92187500034139802, 0.000000000000000000 ) ) ;
#10762 = CARTESIAN_POINT ( 'NONE',  ( -49.99999999999999289, 41.90000000000001279, -16.24598481164531449 ) ) ;
#10763 = CARTESIAN_POINT ( 'NONE',  ( 30.81806926056964002, 46.55937500034139020, 42.41743335407647209 ) ) ;
#10764 = CARTESIAN_POINT ( 'NONE',  ( 9.631387414534489405E-15, 42.42187500034140157, 52.43083105670540789 ) ) ;
#10765 = VECTOR ( 'NONE', #9942, 1000.000000000000000 ) ;
#10766 = VECTOR ( 'NONE', #2882, 1000.000000000000000 ) ;
#10767 = CARTESIAN_POINT ( 'NONE',  ( 50.00000000000000711, 48.90000000000000568, 16.24598481164530739 ) ) ;
#10768 = ORIENTED_EDGE ( 'NONE', *, *, #9148, .T. ) ;
#10769 = CARTESIAN_POINT ( 'NONE',  ( 0.000000000000000000, 193.4213562373095385, 0.000000000000000000 ) ) ;
#10770 = ORIENTED_EDGE ( 'NONE', *, *, #5523, .T. ) ;
#10771 = ORIENTED_EDGE ( 'NONE', *, *, #15459, .F. ) ;
#10772 = CARTESIAN_POINT ( 'NONE',  ( 15.45084971874737789, 28.38125000068279746, 47.55282581475767500 ) ) ;
#10773 = ORIENTED_EDGE ( 'NONE', *, *, #2657, .T. ) ;
#10774 = CIRCLE ( 'NONE', #8920, 50.00000000000000000 ) ;
#10775 = VECTOR ( 'NONE', #3439, 1000.000000000000000 ) ;
#10776 = EDGE_CURVE ( 'NONE', #860, #1083, #7078, .T. ) ;
#10777 = CARTESIAN_POINT ( 'NONE',  ( 30.90169943749473802, 31.08125000068280031, -42.53254041760200721 ) ) ;
#10778 = CARTESIAN_POINT ( 'NONE',  ( -49.86468353125000164, 37.92187500034140157, 0.000000000000000000 ) ) ;
#10779 = CARTESIAN_POINT ( 'NONE',  ( 30.81806926056962936, 21.15937500034140228, -42.41743335407647209 ) ) ;
#10780 = MECHANICAL_DESIGN_GEOMETRIC_PRESENTATION_REPRESENTATION (  '', ( #661 ), #13410 ) ;
#10781 = CARTESIAN_POINT ( 'NONE',  ( 43.87482193696061472, 262.0000000000000000, 10.00000000000000178 ) ) ;
#10782 = SHAPE_DEFINITION_REPRESENTATION ( #3082, #10113 ) ;
#10783 = CARTESIAN_POINT ( 'NONE',  ( 9.657523855033129090E-15, 34.50000000000000711, 52.57311121191334990 ) ) ;
#10784 = EDGE_CURVE ( 'NONE', #8473, #7372, #1219, .T. ) ;
#10785 = EDGE_CURVE ( 'NONE', #9110, #16246, #5170, .T. ) ;
#10786 = CARTESIAN_POINT ( 'NONE',  ( -49.86468353124999453, 41.82187500034140015, -16.20201782572375393 ) ) ;
#10787 = AXIS2_PLACEMENT_3D ( 'NONE', #16239, #9769, #13574 ) ;
#10788 = CARTESIAN_POINT ( 'NONE',  ( 30.90169943749475223, 30.70000000000000284, 42.53254041760199300 ) ) ;
#10789 = AXIS2_PLACEMENT_3D ( 'NONE', #6770, #13147, #12905 ) ;
#10790 = VECTOR ( 'NONE', #8315, 1000.000000000000000 ) ;
#10791 = ORIENTED_EDGE ( 'NONE', *, *, #13129, .T. ) ;
#10792 = AXIS2_PLACEMENT_3D ( 'NONE', #16460, #6241, #2485 ) ;
#10793 = CARTESIAN_POINT ( 'NONE',  ( 30.81806926056962936, 45.22187500034139873, -42.41743335407647209 ) ) ;
#10794 = EDGE_CURVE ( 'NONE', #14575, #11298, #8891, .T. ) ;
#10795 = VERTEX_POINT ( 'NONE', #2574 ) ;
#10796 = ORIENTED_EDGE ( 'NONE', *, *, #13545, .T. ) ;
#10797 = AXIS2_PLACEMENT_3D ( 'NONE', #14182, #15680, #10297 ) ;
#10798 = ORIENTED_EDGE ( 'NONE', *, *, #603, .T. ) ;
#10799 = CARTESIAN_POINT ( 'NONE',  ( -1.240322475938754499E-13, 40.28125000068280315, 50.00000000000000000 ) ) ;
#10800 = DIRECTION ( 'NONE',  ( 0.000000000000000000, 0.000000000000000000, 1.000000000000000000 ) ) ;
#10801 = FACE_BOUND ( 'NONE', #2295, .T. ) ;
#10802 = CARTESIAN_POINT ( 'NONE',  ( 40.45084971874737789, 20.80000000000000426, 29.38926261462365375 ) ) ;
#10803 = CARTESIAN_POINT ( 'NONE',  ( -30.81806926056962226, 44.15937500034139163, 42.41743335407647919 ) ) ;
#10804 = VECTOR ( 'NONE', #6979, 1000.000000000000000 ) ;
#10805 = CARTESIAN_POINT ( 'NONE',  ( 49.86468353125000164, 46.85937500034139447, -6.106662507704105588E-15 ) ) ;
#10806 = CARTESIAN_POINT ( 'NONE',  ( -49.99999999999999289, 30.10000000000000497, 16.24598481164533226 ) ) ;
#10807 = DIRECTION ( 'NONE',  ( 1.000000000000000000, 1.685159948091755373E-14, 0.000000000000000000 ) ) ;
#10808 = DIRECTION ( 'NONE',  ( 0.000000000000000000, 0.000000000000000000, -1.000000000000000000 ) ) ;
#10809 = CARTESIAN_POINT ( 'NONE',  ( -49.99999999999999289, 45.90000000000000568, -16.24598481164531449 ) ) ;
#10810 = CARTESIAN_POINT ( 'NONE',  ( 49.99999999999999289, 22.88125000068280102, -16.24598481164532160 ) ) ;
#10811 = DIRECTION ( 'NONE',  ( 0.000000000000000000, 1.000000000000000000, 0.000000000000000000 ) ) ;
#10812 = ORIENTED_EDGE ( 'NONE', *, *, #5987, .F. ) ;
#10813 = CARTESIAN_POINT ( 'NONE',  ( -49.86468353125000164, 33.85937500034139447, 0.000000000000000000 ) ) ;
#10814 = VERTEX_POINT ( 'NONE', #11312 ) ;
#10815 = ORIENTED_EDGE ( 'NONE', *, *, #6844, .F. ) ;
#10816 = ORIENTED_EDGE ( 'NONE', *, *, #1369, .T. ) ;
#10817 = CIRCLE ( 'NONE', #451, 40.00000000000000000 ) ;
#10818 = CARTESIAN_POINT ( 'NONE',  ( 15.45084971874737789, 44.38125000068279746, 47.55282581475767500 ) ) ;
#10819 = DIRECTION ( 'NONE',  ( -2.312964634635742464E-16, -0.000000000000000000, 1.000000000000000000 ) ) ;
#10820 = CARTESIAN_POINT ( 'NONE',  ( 49.86468353125000164, 20.85937500034139802, -6.106662507704105588E-15 ) ) ;
#10821 = EDGE_LOOP ( 'NONE', ( #15879, #3410, #12272, #8528 ) ) ;
#10822 = DIRECTION ( 'NONE',  ( -0.000000000000000000, -1.000000000000000000, -0.000000000000000000 ) ) ;
#10823 = DIRECTION ( 'NONE',  ( 0.000000000000000000, 0.000000000000000000, 1.000000000000000000 ) ) ;
#10824 = CARTESIAN_POINT ( 'NONE',  ( -3.111920190527341144E-15, 45.28125000068279604, -50.00000000000000000 ) ) ;
#10825 = CARTESIAN_POINT ( 'NONE',  ( -15.40903463028481646, 29.52187500034139589, -47.42413220539093999 ) ) ;
#10826 = CARTESIAN_POINT ( 'NONE',  ( -50.00000000000000000, 48.00000000000000000, 0.000000000000000000 ) ) ;
#10827 = CARTESIAN_POINT ( 'NONE',  ( -2.445080149700054274E-14, 46.50000000000000711, 50.00000000000000000 ) ) ;
#10828 = DIRECTION ( 'NONE',  ( 0.000000000000000000, 1.000000000000000000, 0.000000000000000000 ) ) ;
#10829 = CARTESIAN_POINT ( 'NONE',  ( -49.86468353124999453, 21.82187500034139305, -16.20201782572375393 ) ) ;
#10830 = CARTESIAN_POINT ( 'NONE',  ( 5.026048470455357631, 37.52604847045536474, 39.76282541253124947 ) ) ;
#10831 = CARTESIAN_POINT ( 'NONE',  ( -30.90169943749474868, 31.70000000000000639, -42.53254041760200721 ) ) ;
#10832 = CARTESIAN_POINT ( 'NONE',  ( 49.86468353125000164, 24.85937500034139802, -6.106662507704105588E-15 ) ) ;
#10833 = CARTESIAN_POINT ( 'NONE',  ( 8.446640517145639571E-15, 26.28125000068279959, 50.00000000000000000 ) ) ;
#10834 = EDGE_LOOP ( 'NONE', ( #10241, #16364, #862 ) ) ;
#10835 = CARTESIAN_POINT ( 'NONE',  ( -25.00000000000000355, 287.0000000000000568, -2.499999999999998668 ) ) ;
#10836 = ADVANCED_FACE ( 'NONE', ( #12795 ), #7728, .T. ) ;
#10837 = ORIENTED_EDGE ( 'NONE', *, *, #8778, .F. ) ;
#10838 = DIRECTION ( 'NONE',  ( 0.000000000000000000, 0.000000000000000000, -1.000000000000000000 ) ) ;
#10840 = CARTESIAN_POINT ( 'NONE',  ( 30.81806926056962936, 43.15937500034140584, -42.41743335407647209 ) ) ;
#10839 =( BOUNDED_CURVE ( )  B_SPLINE_CURVE ( 2, ( #13022, #7949, #14172, #6554, #11767, #211, #4219, #764, #7866, #4127, #11614, #5854, #14260 ),
 .UNSPECIFIED., .F., .F. ) 
 B_SPLINE_CURVE_WITH_KNOTS ( ( 3, 2, 2, 2, 2, 2, 3 ),
 ( 0.01666666666666666990, 0.02000000000000000042, 0.02666666666666666838, 0.03333333333333333287, 0.04000000000000000083, 0.04666666666666667573, 0.05000000000000000278 ),
 .UNSPECIFIED. ) 
 CURVE ( )  GEOMETRIC_REPRESENTATION_ITEM ( )  RATIONAL_B_SPLINE_CURVE ( ( 0.9755282581475768211, 0.9755282581475768211, 1.000000000000000000, 0.9510565162951535312, 1.000000000000000000, 0.9510565162951535312, 1.000000000000000000, 0.9510565162951535312, 1.000000000000000000, 0.9510565162951535312, 1.000000000000000000, 0.9755282581475768211, 0.9755282581475768211 ) ) 
 REPRESENTATION_ITEM ( '' )  );
#10841 = CARTESIAN_POINT ( 'NONE',  ( 20.06446087899828967, 286.3455096218830818, 7.532230439496864882 ) ) ;
#10842 = CARTESIAN_POINT ( 'NONE',  ( -20.00000000000000711, 287.0000000000000568, 7.500000000000002665 ) ) ;
#10843 = CARTESIAN_POINT ( 'NONE',  ( 30.81806926056964002, 26.62187500034139731, 42.41743335407647209 ) ) ;
#10844 = CARTESIAN_POINT ( 'NONE',  ( -15.40903463028481646, 33.45937500034139589, -47.42413220539093999 ) ) ;
#10845 = CYLINDRICAL_SURFACE ( 'NONE', #9234, 17.50000000000000000 ) ;
#10846 = CARTESIAN_POINT ( 'NONE',  ( 40.34137639590981195, 33.12187500034139731, -29.30972558990011834 ) ) ;
#10847 = FACE_OUTER_BOUND ( 'NONE', #13258, .T. ) ;
#10848 = CARTESIAN_POINT ( 'NONE',  ( 49.86468353125000164, 42.85937500034140157, -6.106662507704105588E-15 ) ) ;
#10849 = CARTESIAN_POINT ( 'NONE',  ( 15.40903463028481113, 43.32187500034139305, -47.42413220539094709 ) ) ;
#10850 = CARTESIAN_POINT ( 'NONE',  ( -30.81806926056963292, 21.62187500034139376, -42.41743335407647209 ) ) ;
#10851 = ORIENTED_EDGE ( 'NONE', *, *, #11616, .T. ) ;
#10852 = CARTESIAN_POINT ( 'NONE',  ( 9.631387414534489405E-15, 48.35937500034139447, 52.43083105670540789 ) ) ;
#10853 = ORIENTED_EDGE ( 'NONE', *, *, #11624, .F. ) ;
#10854 = ORIENTED_EDGE ( 'NONE', *, *, #407, .F. ) ;
#10855 = CARTESIAN_POINT ( 'NONE',  ( 15.45084971874736723, 31.18125000068279817, -47.55282581475768211 ) ) ;
#10856 = VERTEX_POINT ( 'NONE', #10228 ) ;
#10857 = DIRECTION ( 'NONE',  ( 0.000000000000000000, 1.000000000000000000, 0.000000000000000000 ) ) ;
#10858 = CARTESIAN_POINT ( 'NONE',  ( 40.34137639590981195, 41.12187500034139731, -29.30972558990011834 ) ) ;
#10859 = CARTESIAN_POINT ( 'NONE',  ( -40.34137639590981195, 46.12187500034139731, 29.30972558990012189 ) ) ;
#10860 = CARTESIAN_POINT ( 'NONE',  ( -49.99999999999999289, 39.68125000068280173, -16.24598481164531449 ) ) ;
#10861 = ADVANCED_FACE ( 'NONE', ( #16379, #1317 ), #5014, .F. ) ;
#10862 = EDGE_CURVE ( 'NONE', #11303, #8275, #3911, .T. ) ;
#10863 = APPLICATION_PROTOCOL_DEFINITION ( 'draft international standard', 'automotive_design', 1998, #15337 ) ;
#10864 = CARTESIAN_POINT ( 'NONE',  ( 15.45084971874736723, 39.40000000000000568, -47.55282581475768211 ) ) ;
#10865 = VECTOR ( 'NONE', #4245, 1000.000000000000000 ) ;
#10866 = CARTESIAN_POINT ( 'NONE',  ( -40.34137639590981905, 39.72187500034139873, -29.30972558990011478 ) ) ;
#10867 = DIRECTION ( 'NONE',  ( 1.156482317317871478E-16, 0.000000000000000000, 1.000000000000000000 ) ) ;
#10868 = EDGE_LOOP ( 'NONE', ( #3816, #1875, #4574, #4686 ) ) ;
#10869 = CARTESIAN_POINT ( 'NONE',  ( -15.40903463028481646, 39.52187500034139589, -47.42413220539093999 ) ) ;
#10870 = ORIENTED_EDGE ( 'NONE', *, *, #11634, .F. ) ;
#10871 = ORIENTED_EDGE ( 'NONE', *, *, #3871, .F. ) ;
#10872 = ORIENTED_EDGE ( 'NONE', *, *, #8453, .F. ) ;
#10873 = EDGE_CURVE ( 'NONE', #9033, #13296, #149, .T. ) ;
#10874 = DIRECTION ( 'NONE',  ( 0.000000000000000000, 0.000000000000000000, 1.000000000000000000 ) ) ;
#10875 = CARTESIAN_POINT ( 'NONE',  ( -1.240322475938754499E-13, 40.50000000000000000, 50.00000000000000000 ) ) ;
#10876 = DIRECTION ( 'NONE',  ( 1.000000000000000000, 0.000000000000000000, 0.000000000000000000 ) ) ;
#10877 = CARTESIAN_POINT ( 'NONE',  ( 17.45639740057861644, 21.16801284050037424, 101.0000000000000000 ) ) ;
#10878 = PRESENTATION_LAYER_ASSIGNMENT (  '', '', ( #10358 ) ) ;
#10879 = CARTESIAN_POINT ( 'NONE',  ( 15.40903463028482356, 40.45937500034139589, 47.42413220539093999 ) ) ;
#10880 = DIRECTION ( 'NONE',  ( 0.000000000000000000, 0.000000000000000000, 1.000000000000000000 ) ) ;
#10881 = CARTESIAN_POINT ( 'NONE',  ( 0.000000000000000000, 282.0000000000000000, 88.87749532708107836 ) ) ;
#10882 = FACE_OUTER_BOUND ( 'NONE', #6197, .T. ) ;
#10883 = PLANE ( 'NONE',  #12938 ) ;
#10884 = CARTESIAN_POINT ( 'NONE',  ( 30.90169943749473802, 37.29999999999999716, -42.53254041760200721 ) ) ;
#10885 = CARTESIAN_POINT ( 'NONE',  ( 50.00000000000000000, 37.00000000000000711, -6.123233995736766085E-15 ) ) ;
#10886 = VERTEX_POINT ( 'NONE', #6135 ) ;
#10887 = EDGE_CURVE ( 'NONE', #15132, #14942, #3407, .T. ) ;
#10888 = CARTESIAN_POINT ( 'NONE',  ( 49.86468353125000164, 32.85937500034139447, -6.106662507704105588E-15 ) ) ;
#10889 = EDGE_LOOP ( 'NONE', ( #6420, #8177, #16415, #2560 ) ) ;
#10890 = EDGE_LOOP ( 'NONE', ( #13901, #7722, #5721, #13883 ) ) ;
#10891 = ORIENTED_EDGE ( 'NONE', *, *, #15569, .F. ) ;
#10892 = CARTESIAN_POINT ( 'NONE',  ( -30.90169943749473802, 44.08125000068279320, 42.53254041760200721 ) ) ;
#10893 = CARTESIAN_POINT ( 'NONE',  ( -49.99999999999999289, 40.09999999999999432, 16.24598481164533226 ) ) ;
#10894 = CARTESIAN_POINT ( 'NONE',  ( 40.45084971874737079, 29.19999999999999929, -29.38926261462366440 ) ) ;
#10895 = ORIENTED_EDGE ( 'NONE', *, *, #12457, .F. ) ;
#10896 = CARTESIAN_POINT ( 'NONE',  ( -50.00000000000000000, 38.00000000000000711, 0.000000000000000000 ) ) ;
#10897 = LINE ( 'NONE', #12396, #245 ) ;
#10898 = CARTESIAN_POINT ( 'NONE',  ( -50.00000000000000000, 20.00000000000000000, 0.000000000000000000 ) ) ;
#10899 = PLANE ( 'NONE',  #3896 ) ;
#10900 = DIRECTION ( 'NONE',  ( -0.000000000000000000, -0.000000000000000000, -1.000000000000000000 ) ) ;
#10901 = DIRECTION ( 'NONE',  ( 6.938893903907231459E-18, -1.000000000000000000, -5.551115123125782702E-17 ) ) ;
#10902 = CARTESIAN_POINT ( 'NONE',  ( 15.45084971874736723, 39.40000000000000568, -47.55282581475768211 ) ) ;
#10903 = EDGE_CURVE ( 'NONE', #6731, #4275, #8603, .T. ) ;
#10904 = CARTESIAN_POINT ( 'NONE',  ( 7.919222016226807881, 46.55125428154685352, 50.00000000000000000 ) ) ;
#10905 = CARTESIAN_POINT ( 'NONE',  ( -38.60409515610530917, 20.00000000000000355, 31.77615201968871617 ) ) ;
#10906 = CARTESIAN_POINT ( 'NONE',  ( -49.86468353124999453, 25.82187500034139305, -16.20201782572375393 ) ) ;
#10907 = PLANE ( 'NONE',  #13202 ) ;
#10908 = CARTESIAN_POINT ( 'NONE',  ( -49.99999999999999289, 28.10000000000000497, 16.24598481164533226 ) ) ;
#10909 = CARTESIAN_POINT ( 'NONE',  ( 49.86468353125000164, 22.85937500034139802, -6.106662507704105588E-15 ) ) ;
#10910 = CARTESIAN_POINT ( 'NONE',  ( 40.34137639590981195, 49.05937500034139731, -29.30972558990011834 ) ) ;
#10911 = VERTEX_POINT ( 'NONE', #874 ) ;
#10912 = UNCERTAINTY_MEASURE_WITH_UNIT (LENGTH_MEASURE( 1.000000000000000082E-05 ), #1575, 'distance_accuracy_value', 'NONE');
#10913 = LINE ( 'NONE', #6256, #14989 ) ;
#10914 = ORIENTED_EDGE ( 'NONE', *, *, #4192, .T. ) ;
#10915 = CARTESIAN_POINT ( 'NONE',  ( 7.919222016226822092, 48.55125428154684641, 49.99999999999999289 ) ) ;
#10916 = CARTESIAN_POINT ( 'NONE',  ( -49.86468353124999453, 33.95937500034139589, 16.20201782572377525 ) ) ;
#10917 = CARTESIAN_POINT ( 'NONE',  ( -5.000000000000000000, 102.0000000000000142, -7.580410092413988998 ) ) ;
#10918 = EDGE_CURVE ( 'NONE', #13582, #2974, #7536, .T. ) ;
#10919 = CARTESIAN_POINT ( 'NONE',  ( 30.90169943749475223, 28.48125000068279888, 42.53254041760199300 ) ) ;
#10920 = CARTESIAN_POINT ( 'NONE',  ( -9.189545401991425777, 24.96013318841439599, 101.0000000000000000 ) ) ;
#10921 = CARTESIAN_POINT ( 'NONE',  ( 49.86468353125000164, 30.92187500034139802, -6.106662507704105588E-15 ) ) ;
#10922 = CARTESIAN_POINT ( 'NONE',  ( 40.34137639590981195, 31.05937500034139731, -29.30972558990011834 ) ) ;
#10923 = CARTESIAN_POINT ( 'NONE',  ( -40.45084971874737789, 35.79999999999999716, -29.38926261462365730 ) ) ;
#10924 = CARTESIAN_POINT ( 'NONE',  ( 49.86468353125000164, 30.92187500034139802, -6.106662507704105588E-15 ) ) ;
#10925 = DIRECTION ( 'NONE',  ( 0.9361168066628590134, -0.08189960831908912886, 0.3420201433256691570 ) ) ;
#10926 = CARTESIAN_POINT ( 'NONE',  ( 15.40903463028482356, 46.45937500034139589, 47.42413220539093999 ) ) ;
#10927 = CARTESIAN_POINT ( 'NONE',  ( -3.210462471511496205E-15, 37.42187500034140157, -52.43083105670540789 ) ) ;
#10928 = CARTESIAN_POINT ( 'NONE',  ( 9.631387414534489405E-15, 20.42187500034139802, 52.43083105670540789 ) ) ;
#10930 = ORIENTED_EDGE ( 'NONE', *, *, #6252, .F. ) ;
#10929 =( BOUNDED_CURVE ( )  B_SPLINE_CURVE ( 2, ( #7404, #9817, #743, #5829, #10894, #12473, #15958, #16038, #4665, #16133, #13465, #12221, #4760 ),
 .UNSPECIFIED., .F., .F. ) 
 B_SPLINE_CURVE_WITH_KNOTS ( ( 3, 2, 2, 2, 2, 2, 3 ),
 ( 0.6833333333333333481, 0.6866666666666666474, 0.6933333333333333570, 0.6999999999999999556, 0.7066666666666666652, 0.7133333333333333748, 0.7166666666666666741 ),
 .UNSPECIFIED. ) 
 CURVE ( )  GEOMETRIC_REPRESENTATION_ITEM ( )  RATIONAL_B_SPLINE_CURVE ( ( 0.9755282581475768211, 0.9755282581475768211, 1.000000000000000000, 0.9510565162951535312, 1.000000000000000000, 0.9510565162951535312, 1.000000000000000000, 0.9510565162951535312, 1.000000000000000000, 0.9510565162951535312, 1.000000000000000000, 0.9755282581475768211, 0.9755282581475768211 ) ) 
 REPRESENTATION_ITEM ( '' )  );
#10931 = CARTESIAN_POINT ( 'NONE',  ( -49.86468353125000164, 39.85937500034139447, 0.000000000000000000 ) ) ;
#10932 = ORIENTED_EDGE ( 'NONE', *, *, #1295, .T. ) ;
#10933 = CARTESIAN_POINT ( 'NONE',  ( -49.99999999999999289, 25.88125000068280102, 16.24598481164533226 ) ) ;
#10934 = ORIENTED_EDGE ( 'NONE', *, *, #3807, .T. ) ;
#10935 = CARTESIAN_POINT ( 'NONE',  ( -15.45084971874737256, 35.60000000000000142, -47.55282581475767500 ) ) ;
#10936 = CARTESIAN_POINT ( 'NONE',  ( -30.81806926056963292, 41.62187500034139020, -42.41743335407646498 ) ) ;
#10937 = CARTESIAN_POINT ( 'NONE',  ( -30.81806926056962226, 20.15937500034139518, 42.41743335407647919 ) ) ;
#10938 = CARTESIAN_POINT ( 'NONE',  ( 40.45084971874737079, 31.20000000000000284, -29.38926261462366440 ) ) ;
#10939 = CARTESIAN_POINT ( 'NONE',  ( -49.86468353124999453, 22.02187500034139589, 16.20201782572377525 ) ) ;
#10940 = CONTEXT_DEPENDENT_SHAPE_REPRESENTATION ( #11842, #14082 ) ;
#10941 = CARTESIAN_POINT ( 'NONE',  ( 30.90169943749474157, 35.08125000068278609, -42.53254041760200721 ) ) ;
#10942 = CARTESIAN_POINT ( 'NONE',  ( -40.45084971874737789, 39.80000000000000426, -29.38926261462365730 ) ) ;
#10943 = CARTESIAN_POINT ( 'NONE',  ( -40.34137639590981905, 41.72187500034139873, -29.30972558990011478 ) ) ;
#10944 = DIRECTION ( 'NONE',  ( -1.000000000000000000, 0.000000000000000000, 0.000000000000000000 ) ) ;
#10945 = ORIENTED_EDGE ( 'NONE', *, *, #8288, .F. ) ;
#10946 = CARTESIAN_POINT ( 'NONE',  ( -49.86468353124999453, 44.02187500034139589, 16.20201782572377525 ) ) ;
#10947 = CARTESIAN_POINT ( 'NONE',  ( 2.600676159226420495E-13, 31.28125000068279604, -49.99999999999999289 ) ) ;
#10948 = ORIENTED_EDGE ( 'NONE', *, *, #8775, .F. ) ;
#10949 = VERTEX_POINT ( 'NONE', #13841 ) ;
#10950 = STYLED_ITEM ( 'NONE', ( #16122 ), #14597 ) ;
#10951 = ORIENTED_EDGE ( 'NONE', *, *, #4387, .F. ) ;
#10952 = DIRECTION ( 'NONE',  ( -0.000000000000000000, -1.000000000000000000, -0.000000000000000000 ) ) ;
#10953 = CARTESIAN_POINT ( 'NONE',  ( 12.66515988160610107, 34.57657754388035443, 101.0000000000000000 ) ) ;
#10954 = CARTESIAN_POINT ( 'NONE',  ( -3.111920190527341144E-15, 27.50000000000000000, -50.00000000000000000 ) ) ;
#10955 = CARTESIAN_POINT ( 'NONE',  ( -3.219174618344376363E-15, 21.50000000000000355, -52.57311121191334990 ) ) ;
#10956 = CARTESIAN_POINT ( 'NONE',  ( 49.86468353125001585, 34.75937500034139305, 16.20201782572375038 ) ) ;
#10957 = DIRECTION ( 'NONE',  ( -0.000000000000000000, 1.000000000000000000, -0.000000000000000000 ) ) ;
#10958 = DIRECTION ( 'NONE',  ( 0.000000000000000000, 0.000000000000000000, 1.000000000000000000 ) ) ;
#10959 = CARTESIAN_POINT ( 'NONE',  ( 0.000000000000000000, 217.0000000000000284, 45.00000000000000000 ) ) ;
#10960 = DIRECTION ( 'NONE',  ( 0.000000000000000000, -0.000000000000000000, 1.000000000000000000 ) ) ;
#10961 = CARTESIAN_POINT ( 'NONE',  ( -40.45084971874737789, 45.79999999999999716, -29.38926261462365730 ) ) ;
#10962 = VECTOR ( 'NONE', #14233, 1000.000000000000000 ) ;
#10963 = CARTESIAN_POINT ( 'NONE',  ( 40.45084971874737789, 36.79999999999999716, 29.38926261462365375 ) ) ;
#10964 = CARTESIAN_POINT ( 'NONE',  ( 50.00000000000000711, 36.89999999999999858, 16.24598481164530739 ) ) ;
#10965 = ORIENTED_EDGE ( 'NONE', *, *, #16383, .T. ) ;
#10966 = CARTESIAN_POINT ( 'NONE',  ( 9.631387414534489405E-15, 32.35937500034139447, 52.43083105670540789 ) ) ;
#10967 = ORIENTED_EDGE ( 'NONE', *, *, #5400, .T. ) ;
#10968 = ORIENTED_EDGE ( 'NONE', *, *, #760, .F. ) ;
#10969 = ORIENTED_EDGE ( 'NONE', *, *, #9196, .F. ) ;
#10970 = CARTESIAN_POINT ( 'NONE',  ( -50.00000000000000000, 41.78125000068280315, 0.000000000000000000 ) ) ;
#10971 = CARTESIAN_POINT ( 'NONE',  ( 1.293669679204937499E-13, 39.50000000000000711, -50.00000000000000000 ) ) ;
#10972 = DIRECTION ( 'NONE',  ( 0.000000000000000000, 0.000000000000000000, -1.000000000000000000 ) ) ;
#10974 = ORIENTED_EDGE ( 'NONE', *, *, #10710, .F. ) ;
#10973 = AXIS2_PLACEMENT_3D ( 'NONE', #15529, #313, #6904 ) ;
#10975 = CARTESIAN_POINT ( 'NONE',  ( -7.919222016226802552, 47.33250428222964956, -50.00000000000000000 ) ) ;
#10976 = SURFACE_STYLE_USAGE ( .BOTH. , #8553 ) ;
#10977 = CARTESIAN_POINT ( 'NONE',  ( -1.158672503420370870, 5.028666560261853213, 99.10823753331240482 ) ) ;
#10978 = CARTESIAN_POINT ( 'NONE',  ( -7.499999999999998224, 40.00000000000000711, -24.29058411375428150 ) ) ;
#10979 = FACE_OUTER_BOUND ( 'NONE', #13395, .T. ) ;
#10980 = CYLINDRICAL_SURFACE ( 'NONE', #12171, 50.00000000000000000 ) ;
#10981 = ADVANCED_FACE ( 'NONE', ( #1117 ), #4736, .F. ) ;
#10982 = CARTESIAN_POINT ( 'NONE',  ( -7.919222016226688865, 31.55125428154684286, -50.00000000000003553 ) ) ;
#10983 = CARTESIAN_POINT ( 'NONE',  ( 30.90169943749475223, 46.69999999999999574, 42.53254041760199300 ) ) ;
#10984 = DIRECTION ( 'NONE',  ( -1.000000000000000000, 0.000000000000000000, 0.000000000000000000 ) ) ;
#10985 = CARTESIAN_POINT ( 'NONE',  ( 40.34137639590981195, 21.12187500034139376, -29.30972558990011834 ) ) ;
#10986 = CARTESIAN_POINT ( 'NONE',  ( 0.000000000000000000, 193.4213562373095385, 0.000000000000000000 ) ) ;
#10987 = CARTESIAN_POINT ( 'NONE',  ( 30.90169943749474157, 29.30000000000000071, -42.53254041760200721 ) ) ;
#10988 = CARTESIAN_POINT ( 'NONE',  ( 9.631387414534489405E-15, 26.35937500034140157, 52.43083105670540789 ) ) ;
#10989 = CARTESIAN_POINT ( 'NONE',  ( 8.660254037844387298, 20.00000000000000355, 5.000000000000000000 ) ) ;
#10990 = EDGE_CURVE ( 'NONE', #3473, #15357, #5126, .T. ) ;
#10992 = EDGE_CURVE ( 'NONE', #12352, #7158, #11069, .T. ) ;
#10991 = AXIS2_PLACEMENT_3D ( 'NONE', #3587, #3675, #10316 ) ;
#10993 = CARTESIAN_POINT ( 'NONE',  ( -49.86468353125000164, 47.85937500034139447, 0.000000000000000000 ) ) ;
#10994 = ORIENTED_EDGE ( 'NONE', *, *, #8876, .T. ) ;
#10995 = EDGE_CURVE ( 'NONE', #13460, #13519, #8499, .T. ) ;
#10996 = CARTESIAN_POINT ( 'NONE',  ( 40.34137639590981195, 25.05937500034139376, -29.30972558990011834 ) ) ;
#10997 = EDGE_LOOP ( 'NONE', ( #15188, #3411, #7878, #55 ) ) ;
#10998 = APPLICATION_CONTEXT ( 'automotive_design' ) ;
#10999 = DIRECTION ( 'NONE',  ( 0.000000000000000000, 0.000000000000000000, 1.000000000000000000 ) ) ;
#11000 = CARTESIAN_POINT ( 'NONE',  ( -40.34137639590981195, 38.05937500034139731, 29.30972558990012189 ) ) ;
#11001 = LINE ( 'NONE', #924, #1488 ) ;
#11002 = CARTESIAN_POINT ( 'NONE',  ( 15.45084971874736723, 29.18125000068279817, -47.55282581475768211 ) ) ;
#11003 = CARTESIAN_POINT ( 'NONE',  ( 0.000000000000000000, 267.0000000000000000, -40.00000000000000000 ) ) ;
#11004 = CARTESIAN_POINT ( 'NONE',  ( 15.40903463028482356, 28.52187500034139589, 47.42413220539093999 ) ) ;
#11005 = CARTESIAN_POINT ( 'NONE',  ( -49.86468353124999453, 27.95937500034139944, 16.20201782572377169 ) ) ;
#11006 = CARTESIAN_POINT ( 'NONE',  ( -3.111920190527341144E-15, 35.50000000000000000, -50.00000000000000000 ) ) ;
#11007 = CARTESIAN_POINT ( 'NONE',  ( -40.34137639590981905, 31.72187500034139873, -29.30972558990011478 ) ) ;
#11008 = CARTESIAN_POINT ( 'NONE',  ( 50.00000000000000000, 33.00000000000000000, -6.123233995736766085E-15 ) ) ;
#11009 = CARTESIAN_POINT ( 'NONE',  ( 30.81806926056962936, 45.15937500034139873, -42.41743335407647209 ) ) ;
#11010 = CARTESIAN_POINT ( 'NONE',  ( -3.210462471511496205E-15, 39.42187500034140157, -52.43083105670540789 ) ) ;
#11011 = CARTESIAN_POINT ( 'NONE',  ( -30.81806926056962226, 22.22187500034139163, 42.41743335407647919 ) ) ;
#11012 = ORIENTED_EDGE ( 'NONE', *, *, #12207, .F. ) ;
#11013 = VECTOR ( 'NONE', #15499, 1000.000000000000000 ) ;
#11014 = CARTESIAN_POINT ( 'NONE',  ( -30.81806926056963292, 45.55937500034139731, -42.41743335407646498 ) ) ;
#11015 = ORIENTED_EDGE ( 'NONE', *, *, #5989, .F. ) ;
#11016 = ADVANCED_FACE ( 'NONE', ( #1039 ), #14848, .T. ) ;
#11017 = CARTESIAN_POINT ( 'NONE',  ( 9.657523855033129090E-15, 22.28125000068279959, 52.57311121191334990 ) ) ;
#11018 = ORIENTED_EDGE ( 'NONE', *, *, #9447, .T. ) ;
#11019 = CARTESIAN_POINT ( 'NONE',  ( -1.240322475938754499E-13, 36.50000000000000711, 50.00000000000000000 ) ) ;
#11020 = CARTESIAN_POINT ( 'NONE',  ( -30.81806926056962226, 40.22187500034139873, 42.41743335407647209 ) ) ;
#11021 = CARTESIAN_POINT ( 'NONE',  ( 30.81806926056964002, 20.55937500034139376, 42.41743335407647209 ) ) ;
#11022 = CARTESIAN_POINT ( 'NONE',  ( 30.90169943749473802, 41.30000000000000426, -42.53254041760200721 ) ) ;
#11023 = AXIS2_PLACEMENT_3D ( 'NONE', #8904, #6421, #10407 ) ;
#11024 = CARTESIAN_POINT ( 'NONE',  ( 49.86468353125000164, 20.92187500034139802, -6.106662507704105588E-15 ) ) ;
#11025 = APPLICATION_PROTOCOL_DEFINITION ( 'draft international standard', 'automotive_design', 1998, #6541 ) ;
#11026 = CARTESIAN_POINT ( 'NONE',  ( 49.99999999999999289, 36.88125000068279036, -16.24598481164532160 ) ) ;
#11027 =( BOUNDED_CURVE ( )  B_SPLINE_CURVE ( 2, ( #3571, #8626, #7232, #5990, #11386, #1136, #2315, #6230, #11058, #11301, #16363, #15111, #3736 ),
 .UNSPECIFIED., .F., .T. ) 
 B_SPLINE_CURVE_WITH_KNOTS ( ( 3, 2, 2, 2, 2, 2, 3 ),
 ( 0.05000000000000000278, 0.05333333333333333676, 0.05999999999999999778, 0.06666666666666666574, 0.07333333333333333370, 0.08000000000000000167, 0.08333333333333334259 ),
 .UNSPECIFIED. ) 
 CURVE ( )  GEOMETRIC_REPRESENTATION_ITEM ( )  RATIONAL_B_SPLINE_CURVE ( ( 0.9755282581475768211, 0.9755282581475768211, 1.000000000000000000, 0.9510565162951535312, 1.000000000000000000, 0.9510565162951535312, 1.000000000000000000, 0.9510565162951535312, 1.000000000000000000, 0.9510565162951535312, 1.000000000000000000, 0.9755282581475767101, 0.9755282581475768211 ) ) 
 REPRESENTATION_ITEM ( '' )  );
#11028 = CARTESIAN_POINT ( 'NONE',  ( 40.34137639590981905, 42.72187500034139873, 29.30972558990010768 ) ) ;
#11029 = CARTESIAN_POINT ( 'NONE',  ( -29.67274705320269135, 282.0000000000000000, -11.84549410641580636 ) ) ;
#11030 = ORIENTED_EDGE ( 'NONE', *, *, #12809, .F. ) ;
#11031 = CARTESIAN_POINT ( 'NONE',  ( -49.86468353124999453, 38.02187500034140299, 16.20201782572377525 ) ) ;
#11032 = DIRECTION ( 'NONE',  ( 0.000000000000000000, 0.000000000000000000, -1.000000000000000000 ) ) ;
#11033 = EDGE_LOOP ( 'NONE', ( #8232, #12217, #9051, #5270 ) ) ;
#11034 = ORIENTED_EDGE ( 'NONE', *, *, #12206, .T. ) ;
#11035 = ORIENTED_EDGE ( 'NONE', *, *, #5567, .F. ) ;
#11036 = EDGE_CURVE ( 'NONE', #1977, #5468, #9738, .T. ) ;
#11037 = COLOUR_RGB ( '', 0.66274510, 0.83137255, 0.94901961) ;
#11038 = DIRECTION ( 'NONE',  ( 0.000000000000000000, 0.000000000000000000, -1.000000000000000000 ) ) ;
#11039 = CYLINDRICAL_SURFACE ( 'NONE', #7842, 14.08089297201391155 ) ;
#11040 = CARTESIAN_POINT ( 'NONE',  ( -15.45084971874736368, 22.18125000068279817, 47.55282581475768211 ) ) ;
#11041 = CARTESIAN_POINT ( 'NONE',  ( -40.45084971874737079, 20.20000000000000284, 29.38926261462367151 ) ) ;
#11042 = CARTESIAN_POINT ( 'NONE',  ( 49.86468353124999453, 38.95937500034139589, -16.20201782572376459 ) ) ;
#11043 = CARTESIAN_POINT ( 'NONE',  ( -30.81806926056963292, 49.55937500034139731, -42.41743335407646498 ) ) ;
#11044 = CARTESIAN_POINT ( 'NONE',  ( 0.000000000000000000, 102.0000000000000142, 5.000000000000000000 ) ) ;
#11045 = CARTESIAN_POINT ( 'NONE',  ( -9.642970592016627762, 101.1563493904846780, -1.872989114519522547 ) ) ;
#11046 =( NAMED_UNIT ( * ) SI_UNIT ( $, .STERADIAN. ) SOLID_ANGLE_UNIT ( ) );
#11047 = VECTOR ( 'NONE', #2190, 1000.000000000000000 ) ;
#11049 = DIRECTION ( 'NONE',  ( -0.000000000000000000, -1.000000000000000000, -0.000000000000000000 ) ) ;
#11048 = CIRCLE ( 'NONE', #9470, 7.732050807568878525 ) ;
#11050 = DIRECTION ( 'NONE',  ( 0.000000000000000000, 1.000000000000000000, 0.000000000000000000 ) ) ;
#11051 = VECTOR ( 'NONE', #14809, 1000.000000000000114 ) ;
#11052 = CARTESIAN_POINT ( 'NONE',  ( 49.99999999999999289, 42.88125000068279036, -16.24598481164532160 ) ) ;
#11053 = DIRECTION ( 'NONE',  ( -0.3090169943749448422, -0.9510565162951544194, 0.000000000000000000 ) ) ;
#11054 = PRODUCT_DEFINITION_FORMATION_WITH_SPECIFIED_SOURCE ( 'ANY', '', #4148, .NOT_KNOWN. ) ;
#11055 = ORIENTED_EDGE ( 'NONE', *, *, #2965, .T. ) ;
#11056 = CARTESIAN_POINT ( 'NONE',  ( 15.40903463028482356, 32.45937500034138878, 47.42413220539093999 ) ) ;
#11057 = VECTOR ( 'NONE', #14401, 1000.000000000000000 ) ;
#11058 = CARTESIAN_POINT ( 'NONE',  ( -40.45084971874737789, 47.58125000068280031, -29.38926261462365730 ) ) ;
#11059 = ORIENTED_EDGE ( 'NONE', *, *, #3983, .F. ) ;
#11060 = ORIENTED_EDGE ( 'NONE', *, *, #159, .F. ) ;
#11061 = CARTESIAN_POINT ( 'NONE',  ( 49.99999999999999289, 40.88125000068279036, -16.24598481164532160 ) ) ;
#11062 = VECTOR ( 'NONE', #15308, 1000.000000000000000 ) ;
#11063 = AXIS2_PLACEMENT_3D ( 'NONE', #13869, #12635, #10066 ) ;
#11064 = EDGE_LOOP ( 'NONE', ( #10260, #15594, #13158, #9873 ) ) ;
#11065 = LINE ( 'NONE', #1067, #5451 ) ;
#11066 = CYLINDRICAL_SURFACE ( 'NONE', #3452, 50.00000000000000000 ) ;
#11067 = CARTESIAN_POINT ( 'NONE',  ( 0.000000000000000000, 20.00000000000000355, 0.000000000000000000 ) ) ;
#11068 = DIRECTION ( 'NONE',  ( -0.000000000000000000, 1.000000000000000000, -0.000000000000000000 ) ) ;
#11069 =( BOUNDED_CURVE ( )  B_SPLINE_CURVE ( 2, ( #3387, #8454, #16103, #9793, #13517, #14841, #2121, #11206, #7210, #12271, #4816, #3470, #9869 ),
 .UNSPECIFIED., .F., .F. ) 
 B_SPLINE_CURVE_WITH_KNOTS ( ( 3, 2, 2, 2, 2, 2, 3 ),
 ( 0.1833333333333333481, 0.1866666666666666752, 0.1933333333333333293, 0.2000000000000000111, 0.2066666666666666652, 0.2133333333333333470, 0.2166666666666666741 ),
 .UNSPECIFIED. ) 
 CURVE ( )  GEOMETRIC_REPRESENTATION_ITEM ( )  RATIONAL_B_SPLINE_CURVE ( ( 0.9755282581475767101, 0.9755282581475768211, 1.000000000000000000, 0.9510565162951535312, 1.000000000000000000, 0.9510565162951535312, 1.000000000000000000, 0.9510565162951535312, 1.000000000000000000, 0.9510565162951535312, 1.000000000000000000, 0.9755282581475768211, 0.9755282581475768211 ) ) 
 REPRESENTATION_ITEM ( '' )  );
#11070 = DIRECTION ( 'NONE',  ( 1.000000000000000000, 0.000000000000000000, 0.000000000000000000 ) ) ;
#11071 = FACE_OUTER_BOUND ( 'NONE', #3517, .T. ) ;
#11072 = CARTESIAN_POINT ( 'NONE',  ( -30.90169943749473447, 32.30000000000000426, 42.53254041760200721 ) ) ;
#11073 = DIRECTION ( 'NONE',  ( 0.000000000000000000, 0.000000000000000000, 1.000000000000000000 ) ) ;
#11074 = CARTESIAN_POINT ( 'NONE',  ( -8.880528407616480990, 25.91118970470954963, 101.0000000000000000 ) ) ;
#11075 = CARTESIAN_POINT ( 'NONE',  ( 15.45084971874736723, 47.18125000068280173, -47.55282581475768211 ) ) ;
#11076 = DIRECTION ( 'NONE',  ( 0.08715574274765797158, 0.9961946980917455452, -0.000000000000000000 ) ) ;
#11077 = CARTESIAN_POINT ( 'NONE',  ( -40.45084971874737079, 28.20000000000000284, 29.38926261462367151 ) ) ;
#11078 = VECTOR ( 'NONE', #10742, 1000.000000000000000 ) ;
#11079 = CARTESIAN_POINT ( 'NONE',  ( 40.34137639590981905, 24.65937500034139873, 29.30972558990010768 ) ) ;
#11080 = AXIS2_PLACEMENT_3D ( 'NONE', #8642, #16295, #1073 ) ;
#11081 = CARTESIAN_POINT ( 'NONE',  ( -40.45084971874737079, 41.98125000068279888, 29.38926261462367151 ) ) ;
#11082 = CIRCLE ( 'NONE', #6040, 88.87749532708107836 ) ;
#11083 = CARTESIAN_POINT ( 'NONE',  ( 30.81806926056964002, 48.55937500034138310, 42.41743335407647209 ) ) ;
#11084 = VERTEX_POINT ( 'NONE', #13994 ) ;
#11085 = EDGE_CURVE ( 'NONE', #13440, #10580, #8845, .T. ) ;
#11086 = CARTESIAN_POINT ( 'NONE',  ( -8.477241335952138357, 18.18301270189218855, 102.0000000000000142 ) ) ;
#11087 = VERTEX_POINT ( 'NONE', #13906 ) ;
#11088 = FACE_OUTER_BOUND ( 'NONE', #4941, .T. ) ;
#11089 = CARTESIAN_POINT ( 'NONE',  ( -49.86468353125000164, 35.85937500034140157, 0.000000000000000000 ) ) ;
#11090 = CIRCLE ( 'NONE', #2300, 50.00000000000000000 ) ;
#11091 = CARTESIAN_POINT ( 'NONE',  ( 15.45084971874736723, 41.18125000068280173, -47.55282581475768211 ) ) ;
#11093 = EDGE_CURVE ( 'NONE', #11111, #11502, #6618, .T. ) ;
#11092 = CARTESIAN_POINT ( 'NONE',  ( 9.395693774364776374, 21.00971865127324634, 101.0000000000000000 ) ) ;
#11094 = CARTESIAN_POINT ( 'NONE',  ( -4.336808689942015887E-17, 312.0000000000000568, -2.499999999999999112 ) ) ;
#11096 = EDGE_CURVE ( 'NONE', #4982, #495, #10535, .T. ) ;
#11095 = AXIS2_PLACEMENT_3D ( 'NONE', #7704, #2296, #7462 ) ;
#11097 = DIRECTION ( 'NONE',  ( 0.000000000000000000, 0.000000000000000000, -1.000000000000000000 ) ) ;
#11098 = CARTESIAN_POINT ( 'NONE',  ( -30.81806926056963292, 27.62187500034139731, -42.41743335407647209 ) ) ;
#11099 = CARTESIAN_POINT ( 'NONE',  ( 15.40903463028481113, 27.25937500034139660, -47.42413220539094709 ) ) ;
#11100 = CARTESIAN_POINT ( 'NONE',  ( 40.45084971874737789, 26.58125000068279675, 29.38926261462365375 ) ) ;
#11101 = CARTESIAN_POINT ( 'NONE',  ( -30.81806926056963292, 33.62187500034139731, -42.41743335407646498 ) ) ;
#11102 = DIRECTION ( 'NONE',  ( 0.000000000000000000, 0.000000000000000000, 1.000000000000000000 ) ) ;
#11103 = AXIS2_PLACEMENT_3D ( 'NONE', #5943, #4611, #12501 ) ;
#11104 = EDGE_CURVE ( 'NONE', #15421, #14922, #8178, .T. ) ;
#11105 = CARTESIAN_POINT ( 'NONE',  ( -30.81806926056963292, 43.55937500034139731, -42.41743335407647209 ) ) ;
#11106 = CARTESIAN_POINT ( 'NONE',  ( 49.86468353125000164, 38.92187500034139447, -6.106662507704105588E-15 ) ) ;
#11107 = CARTESIAN_POINT ( 'NONE',  ( -3.210462471511496205E-15, 23.42187500034139802, -52.43083105670540789 ) ) ;
#11108 = EDGE_LOOP ( 'NONE', ( #6478, #5448, #5163, #624 ) ) ;
#11109 = EDGE_CURVE ( 'NONE', #16226, #9644, #8332, .T. ) ;
#11110 = CARTESIAN_POINT ( 'NONE',  ( -49.86468353125000164, 43.85937500034140157, 0.000000000000000000 ) ) ;
#11111 = VERTEX_POINT ( 'NONE', #516 ) ;
#11112 = CARTESIAN_POINT ( 'NONE',  ( 49.99999999999999289, 26.88125000068280102, -16.24598481164532160 ) ) ;
#11113 = VERTEX_POINT ( 'NONE', #5770 ) ;
#11114 = CARTESIAN_POINT ( 'NONE',  ( -30.90169943749474513, 35.69999999999999574, -42.53254041760200721 ) ) ;
#11115 = CARTESIAN_POINT ( 'NONE',  ( 49.86468353125001585, 34.82187500034139305, 16.20201782572375038 ) ) ;
#11116 = AXIS2_PLACEMENT_3D ( 'NONE', #7637, #12703, #1303 ) ;
#11117 = CARTESIAN_POINT ( 'NONE',  ( -3.210462471511496205E-15, 49.42187500034138736, -52.43083105670540789 ) ) ;
#11118 = CARTESIAN_POINT ( 'NONE',  ( 30.90169943749475223, 40.69999999999999574, 42.53254041760199300 ) ) ;
#11119 = CARTESIAN_POINT ( 'NONE',  ( 49.86468353125000164, 24.92187500034139802, -6.106662507704105588E-15 ) ) ;
#11120 = EDGE_CURVE ( 'NONE', #4312, #9544, #10252, .T. ) ;
#11121 = CARTESIAN_POINT ( 'NONE',  ( 9.657523855033129090E-15, 32.28125000068279604, 52.57311121191334990 ) ) ;
#11122 = CARTESIAN_POINT ( 'NONE',  ( 40.34137639590981195, 43.12187500034139731, -29.30972558990011834 ) ) ;
#11123 = CARTESIAN_POINT ( 'NONE',  ( -24.78235906513968345, 286.0218276481963358, -7.282359065137699261 ) ) ;
#11124 = VERTEX_POINT ( 'NONE', #437 ) ;
#11125 = ADVANCED_FACE ( 'NONE', ( #5449 ), #3183, .T. ) ;
#11126 = CARTESIAN_POINT ( 'NONE',  ( 49.86468353124999453, 37.02187500034138878, -16.20201782572376459 ) ) ;
#11127 = CARTESIAN_POINT ( 'NONE',  ( 20.00000000000000711, 284.0710678118654755, -7.499999999999999112 ) ) ;
#11128 = EDGE_LOOP ( 'NONE', ( #977, #6658, #4636, #10054 ) ) ;
#11129 = ORIENTED_EDGE ( 'NONE', *, *, #4751, .T. ) ;
#11130 = ORIENTED_EDGE ( 'NONE', *, *, #7339, .F. ) ;
#11131 = DIRECTION ( 'NONE',  ( 0.7431448254773955764, -0.6691306063588567943, 0.000000000000000000 ) ) ;
#11132 = DIRECTION ( 'NONE',  ( 0.000000000000000000, 1.000000000000000000, 0.000000000000000000 ) ) ;
#11133 = CARTESIAN_POINT ( 'NONE',  ( -15.45084971874736368, 24.18125000068279817, 47.55282581475768211 ) ) ;
#11134 = CARTESIAN_POINT ( 'NONE',  ( 40.34137639590981195, 37.05937500034139731, -29.30972558990011834 ) ) ;
#11135 = CARTESIAN_POINT ( 'NONE',  ( 15.40903463028482356, 42.45937500034140299, 47.42413220539093999 ) ) ;
#11136 = CARTESIAN_POINT ( 'NONE',  ( 30.90169943749473802, 25.30000000000000071, -42.53254041760200721 ) ) ;
#11137 =( BOUNDED_CURVE ( )  B_SPLINE_CURVE ( 2, ( #5727, #967, #2055, #2130, #15772, #804, #7055, #8372, #16109, #13282, #3221, #5808, #12117 ),
 .UNSPECIFIED., .F., .T. ) 
 B_SPLINE_CURVE_WITH_KNOTS ( ( 3, 2, 2, 2, 2, 2, 3 ),
 ( 0.4166666666666666852, 0.4199999999999999845, 0.4266666666666666941, 0.4333333333333333481, 0.4400000000000000022, 0.4466666666666666563, 0.4500000000000000111 ),
 .UNSPECIFIED. ) 
 CURVE ( )  GEOMETRIC_REPRESENTATION_ITEM ( )  RATIONAL_B_SPLINE_CURVE ( ( 0.9755282581475768211, 0.9755282581475770431, 1.000000000000000000, 0.9510565162951535312, 1.000000000000000000, 0.9510565162951535312, 1.000000000000000000, 0.9510565162951535312, 1.000000000000000000, 0.9510565162951535312, 1.000000000000000000, 0.9755282581475765991, 0.9755282581475768211 ) ) 
 REPRESENTATION_ITEM ( '' )  );
#11138 = CARTESIAN_POINT ( 'NONE',  ( -2.500000000000000000, 242.0000000000000284, 47.99999999999999289 ) ) ;
#11139 = AXIS2_PLACEMENT_3D ( 'NONE', #9745, #750, #14702 ) ;
#11140 =( LENGTH_UNIT ( ) NAMED_UNIT ( * ) SI_UNIT ( .MILLI., .METRE. ) );
#11141 = CARTESIAN_POINT ( 'NONE',  ( -49.40314992384925574, 20.00000000000001776, 8.200154929058633968 ) ) ;
#11142 = CARTESIAN_POINT ( 'NONE',  ( 7.919222016226758143, 36.55125428154683931, 50.00000000000000711 ) ) ;
#11143 = CARTESIAN_POINT ( 'NONE',  ( -16.79799753235266735, 27.43226914341395783, 101.0000000000000000 ) ) ;
#11144 = ORIENTED_EDGE ( 'NONE', *, *, #10513, .T. ) ;
#11145 = CARTESIAN_POINT ( 'NONE',  ( 15.40903463028482356, 22.45937500034139589, 47.42413220539093999 ) ) ;
#11146 = ORIENTED_EDGE ( 'NONE', *, *, #760, .T. ) ;
#11147 = VERTEX_POINT ( 'NONE', #9590 ) ;
#11148 = VERTEX_POINT ( 'NONE', #6783 ) ;
#11149 = CARTESIAN_POINT ( 'NONE',  ( 9.657523855033129090E-15, 42.28125000068278894, 52.57311121191334990 ) ) ;
#11150 = VECTOR ( 'NONE', #2152, 1000.000000000000000 ) ;
#11151 = DIRECTION ( 'NONE',  ( -0.000000000000000000, 1.000000000000000000, -0.000000000000000000 ) ) ;
#11152 = FACE_OUTER_BOUND ( 'NONE', #402, .T. ) ;
#11153 = VERTEX_POINT ( 'NONE', #6868 ) ;
#11154 = DIRECTION ( 'NONE',  ( -0.000000000000000000, -1.000000000000000000, -0.000000000000000000 ) ) ;
#11155 = CARTESIAN_POINT ( 'NONE',  ( 17.50000000000000000, 22.50000000000000355, 94.42467108177066848 ) ) ;
#11156 = DIRECTION ( 'NONE',  ( 0.000000000000000000, 0.000000000000000000, -1.000000000000000000 ) ) ;
#11157 = DIRECTION ( 'NONE',  ( -1.000000000000000000, 0.000000000000000000, 0.000000000000000000 ) ) ;
#11158 = CYLINDRICAL_SURFACE ( 'NONE', #7009, 45.00000000000000711 ) ;
#11159 = CARTESIAN_POINT ( 'NONE',  ( -49.86468353125000164, 49.89062500034140157, 0.000000000000000000 ) ) ;
#11160 = DIRECTION ( 'NONE',  ( 0.4999999999999920064, 0.8660254037844432595, 0.000000000000000000 ) ) ;
#11161 = CARTESIAN_POINT ( 'NONE',  ( 1.293669679204937499E-13, 37.28125000068280315, -50.00000000000000000 ) ) ;
#11162 = CARTESIAN_POINT ( 'NONE',  ( -30.90169943749474513, 41.70000000000000284, -42.53254041760200721 ) ) ;
#11163 = CARTESIAN_POINT ( 'NONE',  ( -50.00000000000000000, 43.78125000068280315, 0.000000000000000000 ) ) ;
#11164 = FACE_OUTER_BOUND ( 'NONE', #7034, .T. ) ;
#11165 = VECTOR ( 'NONE', #5752, 1000.000000000000000 ) ;
#11166 = CARTESIAN_POINT ( 'NONE',  ( -40.45084971874737789, 27.80000000000000071, -29.38926261462365730 ) ) ;
#11167 = ADVANCED_FACE ( 'NONE', ( #14470 ), #15655, .T. ) ;
#11168 = CARTESIAN_POINT ( 'NONE',  ( -7.919222016226816763, 25.55125428154684641, -49.99999999999999289 ) ) ;
#11169 = DIRECTION ( 'NONE',  ( 1.000000000000000000, -1.784287003861858895E-15, 0.000000000000000000 ) ) ;
#11170 = CARTESIAN_POINT ( 'NONE',  ( 49.86468353124999453, 42.95937500034139589, -16.20201782572376459 ) ) ;
#11171 = VERTEX_POINT ( 'NONE', #14395 ) ;
#11172 = CARTESIAN_POINT ( 'NONE',  ( -27.07106781186548261, 282.0000000000000000, -6.642135623730948346 ) ) ;
#11173 = EDGE_LOOP ( 'NONE', ( #9565, #13186, #15108, #5129 ) ) ;
#11174 = CARTESIAN_POINT ( 'NONE',  ( 30.90169943749473802, 49.29999999999999716, -42.53254041760200721 ) ) ;
#11175 = CARTESIAN_POINT ( 'NONE',  ( -15.40903463028480580, 32.25937500034140015, 47.42413220539094709 ) ) ;
#11176 = ADVANCED_FACE ( 'NONE', ( #12070 ), #4445, .T. ) ;
#11177 = FACE_OUTER_BOUND ( 'NONE', #16452, .T. ) ;
#11178 = DIRECTION ( 'NONE',  ( -0.2079116908177665590, 0.9781476007338041345, 0.000000000000000000 ) ) ;
#11179 = CARTESIAN_POINT ( 'NONE',  ( -6.668400408272873429E-15, 49.50000000000000000, -50.00000000000000000 ) ) ;
#11180 = LINE ( 'NONE', #7354, #7357 ) ;
#11181 = CARTESIAN_POINT ( 'NONE',  ( 15.40903463028482356, 24.52187500034139589, 47.42413220539093999 ) ) ;
#11182 = CARTESIAN_POINT ( 'NONE',  ( 49.86468353124999453, 26.95937500034139944, -16.20201782572376104 ) ) ;
#11183 = CARTESIAN_POINT ( 'NONE',  ( 30.81806926056964002, 36.62187500034139731, 42.41743335407646498 ) ) ;
#11184 = LINE ( 'NONE', #13404, #9733 ) ;
#11185 = CARTESIAN_POINT ( 'NONE',  ( -30.81806926056963292, 41.55937500034139731, -42.41743335407647209 ) ) ;
#11186 = CARTESIAN_POINT ( 'NONE',  ( -30.81806926056962226, 40.22187500034139873, 42.41743335407647919 ) ) ;
#11187 =( BOUNDED_CURVE ( )  B_SPLINE_CURVE ( 2, ( #13286, #14523, #8220, #5650, #4489, #10716, #394, #11794, #8297, #15777, #9555, #6906, #14286 ),
 .UNSPECIFIED., .F., .F. ) 
 B_SPLINE_CURVE_WITH_KNOTS ( ( 3, 2, 2, 2, 2, 2, 3 ),
 ( 0.5166666666666667185, 0.5200000000000000178, 0.5266666666666666163, 0.5333333333333333259, 0.5400000000000000355, 0.5466666666666666341, 0.5500000000000000444 ),
 .UNSPECIFIED. ) 
 CURVE ( )  GEOMETRIC_REPRESENTATION_ITEM ( )  RATIONAL_B_SPLINE_CURVE ( ( 0.9755282581475768211, 0.9755282581475771542, 1.000000000000000000, 0.9510565162951535312, 1.000000000000000000, 0.9510565162951535312, 1.000000000000000000, 0.9510565162951535312, 1.000000000000000000, 0.9510565162951535312, 1.000000000000000000, 0.9755282581475763770, 0.9755282581475768211 ) ) 
 REPRESENTATION_ITEM ( '' )  );
#11188 = B_SPLINE_CURVE_WITH_KNOTS ( 'NONE', 3,
 ( #422, #1756, #14546, #11736, #2847, #10587, #15472, #14384, #4093, #1908, #15559, #4268, #4188, #14458, #4430, #578, #9333, #3088, #12990, #9254, #10741, #15800, #5672, #9499, #6688, #1594, #3173, #8074 ),
 .UNSPECIFIED., .F., .F.,
 ( 4, 2, 2, 2, 2, 2, 2, 2, 2, 2, 2, 2, 2, 4 ),
 ( 0.01434078593568147847, 0.01607885267100278917, 0.01781691940632409640, 0.02129305287696671781, 0.02303111961228802851, 0.02476918634760933921, 0.02824531981825197102, 0.02998338655357328519, 0.03172145328889459936, 0.03345952002421591354, 0.03519758675953722771, 0.03867372023017986299, 0.04041178696550118410, 0.04214985370082251215 ),
 .UNSPECIFIED. ) ;
#11189 = CARTESIAN_POINT ( 'NONE',  ( -40.45084971874737789, 45.79999999999999716, -29.38926261462365730 ) ) ;
#11190 = ADVANCED_FACE ( 'NONE', ( #4526 ), #14637, .F. ) ;
#11191 = VERTEX_POINT ( 'NONE', #9344 ) ;
#11192 = CARTESIAN_POINT ( 'NONE',  ( 30.81806926056962936, 45.15937500034139873, -42.41743335407646498 ) ) ;
#11193 = ORIENTED_EDGE ( 'NONE', *, *, #4856, .F. ) ;
#11194 = CARTESIAN_POINT ( 'NONE',  ( 50.00000000000000000, 22.78125000068279959, -6.123233995736766085E-15 ) ) ;
#11195 = EDGE_LOOP ( 'NONE', ( #14863, #6036, #4330, #6396, #13578 ) ) ;
#11196 = CARTESIAN_POINT ( 'NONE',  ( 30.90169943749475223, 40.48125000068279888, 42.53254041760199300 ) ) ;
#11197 = CARTESIAN_POINT ( 'NONE',  ( 40.34137639590981195, 43.12187500034139731, -29.30972558990011834 ) ) ;
#11198 = CARTESIAN_POINT ( 'NONE',  ( 30.90169943749473802, 31.30000000000000071, -42.53254041760200721 ) ) ;
#11199 = EDGE_CURVE ( 'NONE', #2051, #3882, #4201, .T. ) ;
#11200 = CARTESIAN_POINT ( 'NONE',  ( -30.81806926056963292, 21.62187500034139376, -42.41743335407647209 ) ) ;
#11201 = CARTESIAN_POINT ( 'NONE',  ( 30.90169943749474157, 31.08125000068280031, -42.53254041760200721 ) ) ;
#11202 = ADVANCED_FACE ( 'NONE', ( #9265 ), #14321, .T. ) ;
#11203 = CARTESIAN_POINT ( 'NONE',  ( -15.40903463028480580, 34.32187500034139305, 47.42413220539094709 ) ) ;
#11204 = CARTESIAN_POINT ( 'NONE',  ( -22.46613188259093974, 283.6958662468272792, -8.733065941307291524 ) ) ;
#11205 = CARTESIAN_POINT ( 'NONE',  ( -15.40903463028481646, 35.52187500034139589, -47.42413220539093999 ) ) ;
#11206 = CARTESIAN_POINT ( 'NONE',  ( -49.99999999999999289, 43.68125000068280173, -16.24598481164531449 ) ) ;
#11207 = VERTEX_POINT ( 'NONE', #11828 ) ;
#11208 = ORIENTED_EDGE ( 'NONE', *, *, #2254, .T. ) ;
#11209 = EDGE_CURVE ( 'NONE', #7494, #16264, #5540, .T. ) ;
#11210 = VERTEX_POINT ( 'NONE', #15728 ) ;
#11211 = DIRECTION ( 'NONE',  ( 0.000000000000000000, 0.000000000000000000, 1.000000000000000000 ) ) ;
#11212 = CARTESIAN_POINT ( 'NONE',  ( 49.99999999999999289, 45.10000000000000142, -16.24598481164532160 ) ) ;
#11213 = CARTESIAN_POINT ( 'NONE',  ( 0.000000000000000000, 193.4213562373095385, 0.000000000000000000 ) ) ;
#11214 = DIRECTION ( 'NONE',  ( 0.000000000000000000, 1.000000000000000000, 0.000000000000000000 ) ) ;
#11215 = CARTESIAN_POINT ( 'NONE',  ( -30.81806926056962226, 36.15937500034139163, 42.41743335407647919 ) ) ;
#11216 = CARTESIAN_POINT ( 'NONE',  ( -30.81806926056963292, 41.55937500034139731, -42.41743335407646498 ) ) ;
#11217 = DIRECTION ( 'NONE',  ( 1.000000000000000000, 0.000000000000000000, 0.000000000000000000 ) ) ;
#11218 = CARTESIAN_POINT ( 'NONE',  ( -17.50000000000000000, 22.50000000000000000, 102.0000000000000142 ) ) ;
#11219 = CARTESIAN_POINT ( 'NONE',  ( -49.99999999999999289, 35.68125000068279462, -16.24598481164531449 ) ) ;
#11220 = EDGE_LOOP ( 'NONE', ( #5825, #14069 ) ) ;
#11221 = CARTESIAN_POINT ( 'NONE',  ( 15.40903463028481113, 23.25937500034139660, -47.42413220539094709 ) ) ;
#11222 = ORIENTED_EDGE ( 'NONE', *, *, #7912, .F. ) ;
#11223 = ORIENTED_EDGE ( 'NONE', *, *, #2024, .T. ) ;
#11224 = ORIENTED_EDGE ( 'NONE', *, *, #2331, .F. ) ;
#11225 = ADVANCED_FACE ( 'NONE', ( #10752, #8256 ), #13160, .T. ) ;
#11226 = ADVANCED_FACE ( 'NONE', ( #14559 ), #13320, .T. ) ;
#11227 = CARTESIAN_POINT ( 'NONE',  ( -40.45084971874737079, 39.98125000068279888, 29.38926261462367151 ) ) ;
#11228 = CARTESIAN_POINT ( 'NONE',  ( -49.99999999999999289, 39.90000000000000568, -16.24598481164531449 ) ) ;
#11229 = LINE ( 'NONE', #11307, #4383 ) ;
#11230 = ORIENTED_EDGE ( 'NONE', *, *, #1165, .F. ) ;
#11231 = CARTESIAN_POINT ( 'NONE',  ( -7.977241335952133916, 17.31698729810774751, 101.0000000000000000 ) ) ;
#11232 = FACE_OUTER_BOUND ( 'NONE', #14009, .T. ) ;
#11233 = DIRECTION ( 'NONE',  ( 1.000000000000000000, 0.000000000000000000, 0.000000000000000000 ) ) ;
#11234 = DIRECTION ( 'NONE',  ( 2.126576849575776229E-17, 0.9848077530122080203, -0.1736481776669307198 ) ) ;
#11235 = CARTESIAN_POINT ( 'NONE',  ( 9.253960653386475815E-15, 98.25246584726779986, -9.080892972013931086 ) ) ;
#11236 = DIRECTION ( 'NONE',  ( 5.069245582283711292E-17, 1.000000000000000000, -8.780190904559502465E-17 ) ) ;
#11238 = FACE_OUTER_BOUND ( 'NONE', #7496, .T. ) ;
#11237 = CIRCLE ( 'NONE', #13858, 10.00000000000000000 ) ;
#11239 =( NAMED_UNIT ( * ) SI_UNIT ( $, .STERADIAN. ) SOLID_ANGLE_UNIT ( ) );
#11240 = CARTESIAN_POINT ( 'NONE',  ( 40.45084971874737079, 49.20000000000000284, -29.38926261462366440 ) ) ;
#11241 = CARTESIAN_POINT ( 'NONE',  ( -49.99999999999999289, 47.88125000068280457, 16.24598481164533226 ) ) ;
#11242 = DIRECTION ( 'NONE',  ( 0.000000000000000000, 0.000000000000000000, -1.000000000000000000 ) ) ;
#11243 = CARTESIAN_POINT ( 'NONE',  ( -50.00000000000000000, 30.00000000000000355, 0.000000000000000000 ) ) ;
#11244 = CARTESIAN_POINT ( 'NONE',  ( -3.210462471511496205E-15, 21.35937500034139092, -52.43083105670540789 ) ) ;
#11245 = CARTESIAN_POINT ( 'NONE',  ( 13.33959974903368995, 33.83821319854147447, 101.0000000000000000 ) ) ;
#11246 = CARTESIAN_POINT ( 'NONE',  ( 30.81806926056962936, 47.15937500034138452, -42.41743335407647209 ) ) ;
#11247 = ORIENTED_EDGE ( 'NONE', *, *, #7662, .T. ) ;
#11248 = CIRCLE ( 'NONE', #13353, 45.00000000000000711 ) ;
#11249 = EDGE_LOOP ( 'NONE', ( #7118, #1878, #10201, #6680 ) ) ;
#11250 = LINE ( 'NONE', #9839, #431 ) ;
#11251 = CARTESIAN_POINT ( 'NONE',  ( -40.34137639590981195, 36.05937500034139731, 29.30972558990012189 ) ) ;
#11252 = EDGE_CURVE ( 'NONE', #2031, #12133, #1005, .T. ) ;
#11253 = EDGE_CURVE ( 'NONE', #6342, #12450, #1796, .T. ) ;
#11254 = CARTESIAN_POINT ( 'NONE',  ( -38.60409515610530917, 20.00000000000000355, 31.77615201968871617 ) ) ;
#11255 = DIRECTION ( 'NONE',  ( 0.8090169943749504489, -0.5877852522924689183, 0.000000000000000000 ) ) ;
#11256 = CARTESIAN_POINT ( 'NONE',  ( 46.06840506420055448, 24.99999999999999289, -19.08445694769665124 ) ) ;
#11257 = CARTESIAN_POINT ( 'NONE',  ( 50.00000000000000000, 46.78125000068279604, -6.123233995736766085E-15 ) ) ;
#11258 = CARTESIAN_POINT ( 'NONE',  ( 9.631387414534489405E-15, 22.42187500034139802, 52.43083105670540789 ) ) ;
#11259 = CARTESIAN_POINT ( 'NONE',  ( -15.40903463028481646, 29.45937500034139589, -47.42413220539093999 ) ) ;
#11260 = DIRECTION ( 'NONE',  ( 1.000000000000000000, 0.000000000000000000, -0.000000000000000000 ) ) ;
#11261 = CARTESIAN_POINT ( 'NONE',  ( 40.34137639590981195, 33.12187500034139731, -29.30972558990011834 ) ) ;
#11262 = CARTESIAN_POINT ( 'NONE',  ( -2.547328955960238000E-13, 30.28125000068279604, 49.99999999999999289 ) ) ;
#11263 = VECTOR ( 'NONE', #15197, 1000.000000000000000 ) ;
#11264 = CARTESIAN_POINT ( 'NONE',  ( 9.657523855033129090E-15, 40.50000000000000711, 52.57311121191334990 ) ) ;
#11265 = CARTESIAN_POINT ( 'NONE',  ( 40.34137639590981905, 38.65937500034139873, 29.30972558990010768 ) ) ;
#11266 = CARTESIAN_POINT ( 'NONE',  ( 49.86468353125001585, 38.82187500034140015, 16.20201782572375038 ) ) ;
#11267 = CARTESIAN_POINT ( 'NONE',  ( -50.00000000000000000, 48.00000000000000000, 0.000000000000000000 ) ) ;
#11268 = VERTEX_POINT ( 'NONE', #7262 ) ;
#11269 = CARTESIAN_POINT ( 'NONE',  ( -3.210462471511496205E-15, 43.35937500034139447, -52.43083105670540789 ) ) ;
#11270 = ORIENTED_EDGE ( 'NONE', *, *, #13663, .T. ) ;
#11271 = CARTESIAN_POINT ( 'NONE',  ( 15.45084971874737789, 24.38125000068279746, 47.55282581475767500 ) ) ;
#11272 = VECTOR ( 'NONE', #9630, 1000.000000000000114 ) ;
#11273 = CARTESIAN_POINT ( 'NONE',  ( 8.477241335952196977, 18.18301270189230578, 101.0000000000000000 ) ) ;
#11274 = CARTESIAN_POINT ( 'NONE',  ( 0.000000000000000000, 22.50000000000000000, 102.0000000000000142 ) ) ;
#11275 = CARTESIAN_POINT ( 'NONE',  ( 30.81806926056962936, 43.22187500034140584, -42.41743335407647209 ) ) ;
#11276 = CARTESIAN_POINT ( 'NONE',  ( 50.00000000000000000, 31.00000000000000355, -6.123233995736766085E-15 ) ) ;
#11277 = CARTESIAN_POINT ( 'NONE',  ( -50.00000000000000000, 50.00000000000000000, 0.000000000000000000 ) ) ;
#11278 = CARTESIAN_POINT ( 'NONE',  ( 50.00000000000000711, 24.68125000068279462, 16.24598481164530739 ) ) ;
#11279 = VECTOR ( 'NONE', #3710, 1000.000000000000000 ) ;
#11280 = CARTESIAN_POINT ( 'NONE',  ( -49.86468353125000164, 33.92187500034139447, 0.000000000000000000 ) ) ;
#11281 = CARTESIAN_POINT ( 'NONE',  ( -25.00000020635302889, 287.0011902442391261, -7.499999664676337829 ) ) ;
#11282 = CARTESIAN_POINT ( 'NONE',  ( -49.86468353125000164, 33.92187500034139447, 0.000000000000000000 ) ) ;
#11283 = ORIENTED_EDGE ( 'NONE', *, *, #606, .T. ) ;
#11284 = EDGE_CURVE ( 'NONE', #14151, #7383, #13563, .T. ) ;
#11285 = ORIENTED_EDGE ( 'NONE', *, *, #8956, .F. ) ;
#11286 = CARTESIAN_POINT ( 'NONE',  ( -7.919222016226688865, 31.55125428154684286, -50.00000000000003553 ) ) ;
#11287 = LINE ( 'NONE', #12775, #9174 ) ;
#11288 = AXIS2_PLACEMENT_3D ( 'NONE', #4942, #13969, #3922 ) ;
#11289 = DIRECTION ( 'NONE',  ( -0.000000000000000000, -1.000000000000000000, -0.000000000000000000 ) ) ;
#11290 = DIRECTION ( 'NONE',  ( -0.8660254037844433705, 0.000000000000000000, -0.4999999999999918399 ) ) ;
#11291 = CARTESIAN_POINT ( 'NONE',  ( 15.40903463028481113, 31.25937500034140015, -47.42413220539094709 ) ) ;
#11292 = EDGE_CURVE ( 'NONE', #8059, #11111, #3626, .T. ) ;
#11293 = CARTESIAN_POINT ( 'NONE',  ( 49.86468353125001585, 48.82187500034139305, 16.20201782572375038 ) ) ;
#11294 = SHAPE_REPRESENTATION_RELATIONSHIP ( 'NONE' , 'NONE' ,  #329, #7430 ) ;
#11295 = DIRECTION ( 'NONE',  ( 0.000000000000000000, 1.000000000000000000, 0.000000000000000000 ) ) ;
#11296 = DIRECTION ( 'NONE',  ( 0.000000000000000000, 0.000000000000000000, 1.000000000000000000 ) ) ;
#11297 = EDGE_CURVE ( 'NONE', #982, #16226, #11250, .T. ) ;
#11298 = VERTEX_POINT ( 'NONE', #14804 ) ;
#11299 = AXIS2_PLACEMENT_3D ( 'NONE', #721, #14675, #10800 ) ;
#11300 = CARTESIAN_POINT ( 'NONE',  ( 30.81806926056964002, 26.55937500034139376, 42.41743335407647209 ) ) ;
#11301 = CARTESIAN_POINT ( 'NONE',  ( -30.90169943749474513, 47.48125000068279888, -42.53254041760200721 ) ) ;
#11302 = VERTEX_POINT ( 'NONE', #9919 ) ;
#11303 = VERTEX_POINT ( 'NONE', #12493 ) ;
#11304 = ADVANCED_FACE ( 'NONE', ( #6019 ), #7349, .T. ) ;
#11305 = CARTESIAN_POINT ( 'NONE',  ( -3.219174618344376363E-15, 39.28125000068279604, -52.57311121191334990 ) ) ;
#11306 = CARTESIAN_POINT ( 'NONE',  ( 7.919222016226693306, 34.33250428222964246, 50.00000000000003553 ) ) ;
#11307 = CARTESIAN_POINT ( 'NONE',  ( 6.123233995736766085E-15, 193.4213562373095385, 50.00000000000000000 ) ) ;
#11308 = ORIENTED_EDGE ( 'NONE', *, *, #13316, .T. ) ;
#11309 = CARTESIAN_POINT ( 'NONE',  ( 5.000000000000000000, 90.58578643762692195, 1.414213562373097588 ) ) ;
#11310 = CARTESIAN_POINT ( 'NONE',  ( -17.44929222242214095, 21.16875962481669760, 101.0000000000000000 ) ) ;
#11311 = CARTESIAN_POINT ( 'NONE',  ( 40.34137639590981195, 49.05937500034139731, -29.30972558990011834 ) ) ;
#11312 = CARTESIAN_POINT ( 'NONE',  ( 5.000000000000000000, 99.58041009241399877, 7.580410092413963241 ) ) ;
#11313 = CARTESIAN_POINT ( 'NONE',  ( -7.919222016226934890, 32.22999571913595673, 49.99999999999996447 ) ) ;
#11314 = PLANE ( 'NONE',  #9007 ) ;
#11315 = VECTOR ( 'NONE', #9901, 1000.000000000000000 ) ;
#11316 = LINE ( 'NONE', #15044, #1204 ) ;
#11317 = AXIS2_PLACEMENT_3D ( 'NONE', #2889, #3972, #6890 ) ;
#11318 = DIRECTION ( 'NONE',  ( 0.000000000000000000, 0.000000000000000000, 1.000000000000000000 ) ) ;
#11319 = CARTESIAN_POINT ( 'NONE',  ( -15.45084971874736368, 46.18125000068280173, 47.55282581475768211 ) ) ;
#11320 = CARTESIAN_POINT ( 'NONE',  ( 49.99999999999999289, 21.09999999999999787, -16.24598481164532160 ) ) ;
#11321 = CARTESIAN_POINT ( 'NONE',  ( 15.45084971874736723, 21.40000000000000213, -47.55282581475768211 ) ) ;
#11322 = CARTESIAN_POINT ( 'NONE',  ( 0.000000000000000000, 267.0000000000000000, -45.00000000000000711 ) ) ;
#11323 = CARTESIAN_POINT ( 'NONE',  ( -3.111920190527341144E-15, 43.50000000000000711, -50.00000000000000000 ) ) ;
#11324 = CARTESIAN_POINT ( 'NONE',  ( -49.86468353125000164, 41.85937500034139447, 0.000000000000000000 ) ) ;
#11325 = AXIS2_PLACEMENT_3D ( 'NONE', #382, #3680, #13721 ) ;
#11326 = ORIENTED_EDGE ( 'NONE', *, *, #11104, .T. ) ;
#11327 = CIRCLE ( 'NONE', #4159, 17.50000000000000000 ) ;
#11329 = EDGE_CURVE ( 'NONE', #8439, #6384, #2169, .T. ) ;
#11328 = VECTOR ( 'NONE', #2375, 1000.000000000000000 ) ;
#11330 = CARTESIAN_POINT ( 'NONE',  ( -7.500000000000000000, 25.00000000000000355, 39.29058411375428506 ) ) ;
#11331 = ORIENTED_EDGE ( 'NONE', *, *, #7836, .F. ) ;
#11332 = CARTESIAN_POINT ( 'NONE',  ( 4.898587196589413026E-15, 267.0000000000000000, 40.00000000000000000 ) ) ;
#11333 = CARTESIAN_POINT ( 'NONE',  ( -49.86468353125000164, 27.85937500034139447, 0.000000000000000000 ) ) ;
#11334 = CARTESIAN_POINT ( 'NONE',  ( -3.111920190527341144E-15, 35.28125000068280315, -50.00000000000000000 ) ) ;
#11335 = CARTESIAN_POINT ( 'NONE',  ( -50.00000000000000000, 49.78125000068280315, 0.000000000000000000 ) ) ;
#11336 = CARTESIAN_POINT ( 'NONE',  ( 46.44184698740882311, 25.00000000000000000, -18.15679736478467987 ) ) ;
#11337 = CARTESIAN_POINT ( 'NONE',  ( 7.919222016226693306, 30.33250428222964246, 50.00000000000003553 ) ) ;
#11338 = CARTESIAN_POINT ( 'NONE',  ( -15.40903463028480580, 24.32187500034139660, 47.42413220539094709 ) ) ;
#11339 = CARTESIAN_POINT ( 'NONE',  ( -3.210462471511496205E-15, 25.35937500034139802, -52.43083105670540789 ) ) ;
#11340 = CIRCLE ( 'NONE', #12927, 40.00000000000000000 ) ;
#11341 = DIRECTION ( 'NONE',  ( 0.000000000000000000, -0.000000000000000000, 1.000000000000000000 ) ) ;
#11342 = CARTESIAN_POINT ( 'NONE',  ( 40.34137639590981905, 34.72187500034139873, 29.30972558990010768 ) ) ;
#11343 = AXIS2_PLACEMENT_3D ( 'NONE', #8632, #2229, #12472 ) ;
#11344 = FACE_OUTER_BOUND ( 'NONE', #3687, .T. ) ;
#11345 = CARTESIAN_POINT ( 'NONE',  ( -30.90169943749473802, 34.29999999999998295, 42.53254041760200721 ) ) ;
#11346 = CARTESIAN_POINT ( 'NONE',  ( -49.86468353125000164, 39.85937500034139447, 0.000000000000000000 ) ) ;
#11347 = CARTESIAN_POINT ( 'NONE',  ( 49.86468353125001585, 28.82187500034139305, 16.20201782572375038 ) ) ;
#11348 = CARTESIAN_POINT ( 'NONE',  ( 9.657523855033129090E-15, 46.50000000000000711, 52.57311121191334990 ) ) ;
#11349 = ADVANCED_FACE ( 'NONE', ( #11088 ), #3098, .T. ) ;
#11350 = ORIENTED_EDGE ( 'NONE', *, *, #3232, .F. ) ;
#11351 = CARTESIAN_POINT ( 'NONE',  ( 15.40903463028482356, 36.45937500034139589, 47.42413220539093999 ) ) ;
#11352 = VECTOR ( 'NONE', #15127, 1000.000000000000000 ) ;
#11353 = ORIENTED_EDGE ( 'NONE', *, *, #8853, .T. ) ;
#11354 = CARTESIAN_POINT ( 'NONE',  ( 24.96465690379595515, 286.9981936728412393, -7.464656903795367171 ) ) ;
#11355 = CARTESIAN_POINT ( 'NONE',  ( 15.40903463028481113, 45.25937500034140015, -47.42413220539094709 ) ) ;
#11356 = CARTESIAN_POINT ( 'NONE',  ( -15.45084971874737256, 33.60000000000000142, -47.55282581475767500 ) ) ;
#11357 = CARTESIAN_POINT ( 'NONE',  ( 40.34137639590981195, 25.12187500034139376, -29.30972558990011834 ) ) ;
#11358 = CARTESIAN_POINT ( 'NONE',  ( 0.000000000000000000, 52.00000000000000711, 0.000000000000000000 ) ) ;
#11359 = CARTESIAN_POINT ( 'NONE',  ( -3.210462471511496205E-15, 43.42187500034140157, -52.43083105670540789 ) ) ;
#11360 = CARTESIAN_POINT ( 'NONE',  ( -30.90169943749473447, 26.08125000068279320, 42.53254041760200721 ) ) ;
#11361 = CARTESIAN_POINT ( 'NONE',  ( 15.45084971874736723, 49.39999999999999858, -47.55282581475768211 ) ) ;
#11362 = CARTESIAN_POINT ( 'NONE',  ( 40.45084971874737789, 30.58125000068279675, 29.38926261462365375 ) ) ;
#11363 = CARTESIAN_POINT ( 'NONE',  ( -15.40903463028481646, 49.52187500034140299, -47.42413220539093999 ) ) ;
#11364 = CARTESIAN_POINT ( 'NONE',  ( -40.34137639590981195, 32.12187500034140442, 29.30972558990012189 ) ) ;
#11365 = CARTESIAN_POINT ( 'NONE',  ( -26.78441608355137049, 282.9883952696293932, -9.284416083551363386 ) ) ;
#11366 = DIRECTION ( 'NONE',  ( 0.000000000000000000, 0.000000000000000000, 1.000000000000000000 ) ) ;
#11367 = ORIENTED_EDGE ( 'NONE', *, *, #7745, .F. ) ;
#11368 = AXIS2_PLACEMENT_3D ( 'NONE', #9550, #13604, #9466 ) ;
#11369 = ORIENTED_EDGE ( 'NONE', *, *, #13093, .F. ) ;
#11370 = CARTESIAN_POINT ( 'NONE',  ( 9.395693774364776374, 21.00971865127324634, 102.0000000000000142 ) ) ;
#11371 = CARTESIAN_POINT ( 'NONE',  ( 40.45084971874737079, 45.20000000000000284, -29.38926261462366440 ) ) ;
#11372 =( BOUNDED_CURVE ( )  B_SPLINE_CURVE ( 2, ( #14168, #10442, #12771, #14006, #16434, #2625, #10199, #1290, #9109, #285, #4123, #11610, #2702 ),
 .UNSPECIFIED., .F., .F. ) 
 B_SPLINE_CURVE_WITH_KNOTS ( ( 3, 2, 2, 2, 2, 2, 3 ),
 ( 0.7166666666666666741, 0.7199999999999999734, 0.7266666666666666829, 0.7333333333333332815, 0.7399999999999999911, 0.7466666666666667007, 0.7500000000000000000 ),
 .UNSPECIFIED. ) 
 CURVE ( )  GEOMETRIC_REPRESENTATION_ITEM ( )  RATIONAL_B_SPLINE_CURVE ( ( 0.9755282581475768211, 0.9755282581475768211, 1.000000000000000000, 0.9510565162951535312, 1.000000000000000000, 0.9510565162951535312, 1.000000000000000000, 0.9510565162951535312, 1.000000000000000000, 0.9510565162951535312, 1.000000000000000000, 0.9755282581475768211, 0.9755282581475768211 ) ) 
 REPRESENTATION_ITEM ( '' )  );
#11373 = EDGE_CURVE ( 'NONE', #11702, #14824, #10273, .T. ) ;
#11374 = CARTESIAN_POINT ( 'NONE',  ( 0.000000000000000000, 217.0000000000000284, 0.000000000000000000 ) ) ;
#11375 = DIRECTION ( 'NONE',  ( 0.000000000000000000, 1.000000000000000000, 0.000000000000000000 ) ) ;
#11376 = EDGE_CURVE ( 'NONE', #3456, #1328, #15824, .T. ) ;
#11377 = CARTESIAN_POINT ( 'NONE',  ( 15.40903463028482356, 32.45937500034138878, 47.42413220539093999 ) ) ;
#11378 = CARTESIAN_POINT ( 'NONE',  ( -3.210462471511496205E-15, 43.42187500034140157, -52.43083105670540789 ) ) ;
#11379 = CARTESIAN_POINT ( 'NONE',  ( -15.45084971874737256, 39.60000000000000142, -47.55282581475767500 ) ) ;
#11380 = EDGE_CURVE ( 'NONE', #10383, #13787, #1491, .T. ) ;
#11381 = CARTESIAN_POINT ( 'NONE',  ( 0.000000000000000000, 262.0000000000000000, 45.00000000000000000 ) ) ;
#11382 = CARTESIAN_POINT ( 'NONE',  ( 38.60409515610501074, 25.00000000000000000, -31.77615201968907144 ) ) ;
#11383 = ORIENTED_EDGE ( 'NONE', *, *, #8247, .F. ) ;
#11384 = CARTESIAN_POINT ( 'NONE',  ( 30.81806926056964002, 22.55937500034139020, 42.41743335407647209 ) ) ;
#11385 = VERTEX_POINT ( 'NONE', #13484 ) ;
#11386 = CARTESIAN_POINT ( 'NONE',  ( -40.45084971874737079, 47.98125000068279888, 29.38926261462367151 ) ) ;
#11387 = EDGE_CURVE ( 'NONE', #4712, #11650, #11864, .T. ) ;
#11388 = ORIENTED_EDGE ( 'NONE', *, *, #11199, .T. ) ;
#11389 = ORIENTED_EDGE ( 'NONE', *, *, #9698, .T. ) ;
#11390 = FACE_OUTER_BOUND ( 'NONE', #7865, .T. ) ;
#11391 = DIRECTION ( 'NONE',  ( 0.000000000000000000, 0.000000000000000000, -1.000000000000000000 ) ) ;
#11392 = PLANE ( 'NONE',  #3984 ) ;
#11393 = CIRCLE ( 'NONE', #4228, 24.08089297201390977 ) ;
#11394 = CARTESIAN_POINT ( 'NONE',  ( 30.90169943749473802, 33.08125000068279320, -42.53254041760200721 ) ) ;
#11395 = DIRECTION ( 'NONE',  ( 0.000000000000000000, 0.000000000000000000, -1.000000000000000000 ) ) ;
#11396 = DIRECTION ( 'NONE',  ( 0.000000000000000000, 0.000000000000000000, -1.000000000000000000 ) ) ;
#11397 = DIRECTION ( 'NONE',  ( 0.000000000000000000, 0.000000000000000000, 1.000000000000000000 ) ) ;
#11398 = CARTESIAN_POINT ( 'NONE',  ( -15.45084971874737256, 49.60000000000000853, -47.55282581475767500 ) ) ;
#11399 = CARTESIAN_POINT ( 'NONE',  ( 49.99999999999999289, 44.88125000068279036, -16.24598481164532160 ) ) ;
#11400 = CARTESIAN_POINT ( 'NONE',  ( 50.00000000000000000, 44.78125000068280315, -6.123233995736766085E-15 ) ) ;
#11401 = ADVANCED_FACE ( 'NONE', ( #2006 ), #7103, .F. ) ;
#11402 = CARTESIAN_POINT ( 'NONE',  ( 40.45084971874737079, 21.19999999999999929, -29.38926261462366440 ) ) ;
#11403 = CARTESIAN_POINT ( 'NONE',  ( -49.86468353124999453, 21.95937500034138878, 16.20201782572377525 ) ) ;
#11404 = VERTEX_POINT ( 'NONE', #16059 ) ;
#11405 = CARTESIAN_POINT ( 'NONE',  ( 30.81806926056962936, 41.15937500034139873, -42.41743335407647209 ) ) ;
#11406 = PRESENTATION_LAYER_ASSIGNMENT (  '', '', ( #2096 ) ) ;
#11407 = EDGE_LOOP ( 'NONE', ( #2607, #2123, #12380, #12045, #15407, #7661 ) ) ;
#11408 = EDGE_CURVE ( 'NONE', #14050, #14905, #4691, .T. ) ;
#11409 = DIRECTION ( 'NONE',  ( 1.000000000000000000, 0.000000000000000000, 0.000000000000000000 ) ) ;
#11410 = ORIENTED_EDGE ( 'NONE', *, *, #832, .T. ) ;
#11411 = CARTESIAN_POINT ( 'NONE',  ( 7.499999999999998224, 40.00000000000000711, 24.29058411375428150 ) ) ;
#11412 = CARTESIAN_POINT ( 'NONE',  ( -40.34137639590981195, 32.05937500034139731, 29.30972558990012189 ) ) ;
#11413 = EDGE_CURVE ( 'NONE', #2743, #12041, #2590, .T. ) ;
#11414 = CARTESIAN_POINT ( 'NONE',  ( 0.000000000000000000, 54.00000000000000711, 63.16733765196516970 ) ) ;
#11415 = DIRECTION ( 'NONE',  ( -0.000000000000000000, 1.000000000000000000, -0.000000000000000000 ) ) ;
#11416 = CARTESIAN_POINT ( 'NONE',  ( 47.79496856443405761, 24.99999999999999289, -14.21716018044656238 ) ) ;
#11417 = CARTESIAN_POINT ( 'NONE',  ( -49.86468353125000164, 35.92187500034140157, 0.000000000000000000 ) ) ;
#11418 = DIRECTION ( 'NONE',  ( 0.000000000000000000, 0.000000000000000000, 1.000000000000000000 ) ) ;
#11419 = CARTESIAN_POINT ( 'NONE',  ( 49.86468353125001585, 24.75937500034139660, 16.20201782572375038 ) ) ;
#11420 = PLANE ( 'NONE',  #14243 ) ;
#11421 = CARTESIAN_POINT ( 'NONE',  ( 15.40903463028482356, 38.52187500034139589, 47.42413220539093999 ) ) ;
#11422 = CARTESIAN_POINT ( 'NONE',  ( -2.500000000000000000, 247.0000000000000284, -47.99999999999999289 ) ) ;
#11423 = CARTESIAN_POINT ( 'NONE',  ( -49.99999999999999289, 29.89999999999999858, -16.24598481164531449 ) ) ;
#11424 = CARTESIAN_POINT ( 'NONE',  ( -30.81806926056963292, 37.55937500034139020, -42.41743335407647209 ) ) ;
#11425 = CARTESIAN_POINT ( 'NONE',  ( 30.81806926056964002, 34.62187500034139731, 42.41743335407647209 ) ) ;
#11426 = CARTESIAN_POINT ( 'NONE',  ( -30.90169943749474868, 47.70000000000000995, -42.53254041760200721 ) ) ;
#11427 = ORIENTED_EDGE ( 'NONE', *, *, #13650, .T. ) ;
#11428 = ORIENTED_EDGE ( 'NONE', *, *, #6418, .F. ) ;
#11429 = CARTESIAN_POINT ( 'NONE',  ( 49.86468353124999453, 34.95937500034138878, -16.20201782572376104 ) ) ;
#11430 = ORIENTED_EDGE ( 'NONE', *, *, #5900, .T. ) ;
#11431 = VERTEX_POINT ( 'NONE', #3839 ) ;
#11432 = EDGE_CURVE ( 'NONE', #13826, #9838, #11082, .T. ) ;
#11433 = CARTESIAN_POINT ( 'NONE',  ( 24.76951992798385760, 286.3033656649012642, -7.269519927984439356 ) ) ;
#11434 = CARTESIAN_POINT ( 'NONE',  ( 40.34137639590981195, 45.05937500034139731, -29.30972558990011834 ) ) ;
#11435 = CARTESIAN_POINT ( 'NONE',  ( 9.395693774364776374, 21.00971865127324634, 102.0000000000000142 ) ) ;
#11436 = CARTESIAN_POINT ( 'NONE',  ( -3.210462471511496205E-15, 21.42187500034139802, -52.43083105670540789 ) ) ;
#11437 = DIRECTION ( 'NONE',  ( 0.000000000000000000, 1.000000000000000000, 0.000000000000000000 ) ) ;
#11438 = CARTESIAN_POINT ( 'NONE',  ( 49.86468353124999453, 45.02187500034138878, -16.20201782572376459 ) ) ;
#11439 = DIRECTION ( 'NONE',  ( 0.000000000000000000, 0.000000000000000000, 1.000000000000000000 ) ) ;
#11440 = CARTESIAN_POINT ( 'NONE',  ( 50.00000000000000000, 47.00000000000000000, -6.123233995736766085E-15 ) ) ;
#11441 = CARTESIAN_POINT ( 'NONE',  ( 40.45084971874737789, 26.58125000068279675, 29.38926261462365375 ) ) ;
#11442 = CARTESIAN_POINT ( 'NONE',  ( 17.50000000000000000, 22.50000000000000355, 94.42467108177066848 ) ) ;
#11443 = CARTESIAN_POINT ( 'NONE',  ( -49.86468353124999453, 33.82187500034138594, -16.20201782572375393 ) ) ;
#11444 = CARTESIAN_POINT ( 'NONE',  ( -25.00000000000001066, 287.0000000000000000, -7.500000000000000888 ) ) ;
#11445 = DIRECTION ( 'NONE',  ( 0.000000000000000000, -0.000000000000000000, 1.000000000000000000 ) ) ;
#11446 = ORIENTED_EDGE ( 'NONE', *, *, #10618, .F. ) ;
#11447 = VERTEX_POINT ( 'NONE', #12810 ) ;
#11448 = LINE ( 'NONE', #11370, #7595 ) ;
#11449 = DIRECTION ( 'NONE',  ( -0.9135454576426004225, -0.4067366430758009854, 0.000000000000000000 ) ) ;
#11450 = CARTESIAN_POINT ( 'NONE',  ( -49.99999999999999289, 23.90000000000000213, -16.24598481164531449 ) ) ;
#11451 = DIRECTION ( 'NONE',  ( -0.000000000000000000, 1.000000000000000000, -0.000000000000000000 ) ) ;
#11452 = CARTESIAN_POINT ( 'NONE',  ( 40.34137639590981195, 31.05937500034139731, -29.30972558990011834 ) ) ;
#11453 = CARTESIAN_POINT ( 'NONE',  ( 9.631387414534489405E-15, 46.42187500034139447, 52.43083105670540789 ) ) ;
#11454 = CYLINDRICAL_SURFACE ( 'NONE', #2213, 10.00000000000000000 ) ;
#11455 = CARTESIAN_POINT ( 'NONE',  ( 5.000000000000000000, 126.6482322781408953, -36.06244584051386681 ) ) ;
#11456 = DIRECTION ( 'NONE',  ( 0.1045284632676572456, -0.9945218953682730678, -0.000000000000000000 ) ) ;
#11457 = ORIENTED_EDGE ( 'NONE', *, *, #10862, .T. ) ;
#11458 = CARTESIAN_POINT ( 'NONE',  ( -3.210462471511496205E-15, 23.35937500034139802, -52.43083105670540789 ) ) ;
#11459 = ORIENTED_EDGE ( 'NONE', *, *, #9573, .T. ) ;
#11460 = CARTESIAN_POINT ( 'NONE',  ( -49.99999999999999289, 45.88125000068279746, 16.24598481164533226 ) ) ;
#11461 = EDGE_LOOP ( 'NONE', ( #5100, #9701, #962, #6417 ) ) ;
#11462 = ORIENTED_EDGE ( 'NONE', *, *, #15446, .T. ) ;
#11463 =( BOUNDED_CURVE ( )  B_SPLINE_CURVE ( 3, ( #3420, #15041, #9982, #6089 ),
 .UNSPECIFIED., .F., .F. ) 
 B_SPLINE_CURVE_WITH_KNOTS ( ( 4, 4 ),
 ( 0.000000000000000000, 1.570796326794896558 ),
 .UNSPECIFIED. ) 
 CURVE ( )  GEOMETRIC_REPRESENTATION_ITEM ( )  RATIONAL_B_SPLINE_CURVE ( ( 1.000000000000000000, 0.8047378541243649375, 0.8047378541243649375, 1.000000000000000000 ) ) 
 REPRESENTATION_ITEM ( '' )  );
#11464 = CARTESIAN_POINT ( 'NONE',  ( 30.90169943749475223, 34.48125000068279888, 42.53254041760199300 ) ) ;
#11465 = CARTESIAN_POINT ( 'NONE',  ( 1.293669679204937499E-13, 39.28125000068280315, -50.00000000000000000 ) ) ;
#11466 = DIRECTION ( 'NONE',  ( 0.000000000000000000, 0.000000000000000000, -1.000000000000000000 ) ) ;
#11467 = CARTESIAN_POINT ( 'NONE',  ( 50.00000000000000000, 32.78125000068279604, -6.123233995736766085E-15 ) ) ;
#11468 = CARTESIAN_POINT ( 'NONE',  ( 24.99999999999999645, 287.0000000000000568, 2.500000000000003109 ) ) ;
#11469 = DIRECTION ( 'NONE',  ( 0.000000000000000000, 0.000000000000000000, 1.000000000000000000 ) ) ;
#11470 = CARTESIAN_POINT ( 'NONE',  ( 49.99999999999999289, 24.88125000068279746, -16.24598481164532160 ) ) ;
#11471 = FILL_AREA_STYLE ('',( #11548 ) ) ;
#11472 = CARTESIAN_POINT ( 'NONE',  ( -40.45084971874737789, 49.80000000000000426, -29.38926261462365730 ) ) ;
#11473 = CARTESIAN_POINT ( 'NONE',  ( -15.45084971874737256, 41.38125000068279746, -47.55282581475767500 ) ) ;
#11474 = CARTESIAN_POINT ( 'NONE',  ( -3.111920190527341144E-15, 45.28125000068279604, -50.00000000000000000 ) ) ;
#11475 = CARTESIAN_POINT ( 'NONE',  ( 40.45084971874737079, 46.98125000068280599, -29.38926261462366440 ) ) ;
#11476 = LINE ( 'NONE', #7815, #12121 ) ;
#11477 = ORIENTED_EDGE ( 'NONE', *, *, #8203, .F. ) ;
#11478 = CARTESIAN_POINT ( 'NONE',  ( 49.86468353124999453, 46.95937500034139589, -16.20201782572376459 ) ) ;
#11479 = ORIENTED_EDGE ( 'NONE', *, *, #13723, .T. ) ;
#11480 = FACE_OUTER_BOUND ( 'NONE', #817, .T. ) ;
#11481 = PLANE ( 'NONE',  #2029 ) ;
#11482 = CARTESIAN_POINT ( 'NONE',  ( -30.81806926056962226, 32.15937500034139873, 42.41743335407647919 ) ) ;
#11483 = EDGE_CURVE ( 'NONE', #12652, #2769, #13807, .T. ) ;
#11485 = ORIENTED_EDGE ( 'NONE', *, *, #6509, .F. ) ;
#11484 = AXIS2_PLACEMENT_3D ( 'NONE', #9217, #11456, #301 ) ;
#11486 = DIRECTION ( 'NONE',  ( -0.000000000000000000, -1.000000000000000000, -0.000000000000000000 ) ) ;
#11487 = DIRECTION ( 'NONE',  ( -0.000000000000000000, 1.000000000000000000, -0.000000000000000000 ) ) ;
#11488 = CARTESIAN_POINT ( 'NONE',  ( 47.18644234407140203, 25.00000000000000711, -16.12223069495473737 ) ) ;
#11489 = CARTESIAN_POINT ( 'NONE',  ( 40.34137639590981905, 36.72187500034139163, 29.30972558990010768 ) ) ;
#11490 = CARTESIAN_POINT ( 'NONE',  ( 17.35186893731097868, 20.17349094513210161, 102.0000000000000142 ) ) ;
#11491 = CARTESIAN_POINT ( 'NONE',  ( 40.34137639590981905, 24.65937500034139873, 29.30972558990010768 ) ) ;
#11492 = CARTESIAN_POINT ( 'NONE',  ( -5.000000000000000000, 99.58041009241398456, 7.580410092413952583 ) ) ;
#11493 = CARTESIAN_POINT ( 'NONE',  ( -40.34137639590981195, 26.12187500034139731, 29.30972558990012189 ) ) ;
#11494 = ADVANCED_FACE ( 'NONE', ( #5184 ), #6423, .F. ) ;
#11495 = CARTESIAN_POINT ( 'NONE',  ( -9.395693774364753281, 21.00971865127312199, 101.0000000000000000 ) ) ;
#11496 = ADVANCED_FACE ( 'NONE', ( #13884 ), #7821, .F. ) ;
#11497 = CARTESIAN_POINT ( 'NONE',  ( -3.219174618344376363E-15, 33.50000000000000711, -52.57311121191334990 ) ) ;
#11498 = CARTESIAN_POINT ( 'NONE',  ( -40.34137639590981195, 36.05937500034139731, 29.30972558990012189 ) ) ;
#11499 = CARTESIAN_POINT ( 'NONE',  ( 40.34137639590981905, 30.72187500034139518, 29.30972558990010768 ) ) ;
#11500 = CARTESIAN_POINT ( 'NONE',  ( 40.45084971874737079, 41.20000000000000284, -29.38926261462366440 ) ) ;
#11501 = ORIENTED_EDGE ( 'NONE', *, *, #14515, .T. ) ;
#11502 = VERTEX_POINT ( 'NONE', #14130 ) ;
#11503 = CARTESIAN_POINT ( 'NONE',  ( -3.210462471511496205E-15, 33.35937500034139447, -52.43083105670540789 ) ) ;
#11504 = ORIENTED_EDGE ( 'NONE', *, *, #15379, .F. ) ;
#11505 = EDGE_LOOP ( 'NONE', ( #5554, #8390, #5591, #5985 ) ) ;
#11506 = CARTESIAN_POINT ( 'NONE',  ( 29.34550962211230640, 282.0322304394513253, -11.19101924422353811 ) ) ;
#11507 = CARTESIAN_POINT ( 'NONE',  ( 49.86468353125000164, 48.85937500034139447, -6.106662507704105588E-15 ) ) ;
#11508 = FACE_BOUND ( 'NONE', #714, .T. ) ;
#11509 = CARTESIAN_POINT ( 'NONE',  ( -49.86468353125000164, 25.92187500034139802, 0.000000000000000000 ) ) ;
#11510 = VECTOR ( 'NONE', #13714, 1000.000000000000000 ) ;
#11511 = CARTESIAN_POINT ( 'NONE',  ( -30.00000000000000711, 282.0000000000000000, 12.50000000000000000 ) ) ;
#11512 = CARTESIAN_POINT ( 'NONE',  ( 49.86468353125000164, 44.92187500034140157, -6.106662507704105588E-15 ) ) ;
#11513 = CARTESIAN_POINT ( 'NONE',  ( -30.81806926056963292, 43.55937500034139731, -42.41743335407646498 ) ) ;
#11514 = LINE ( 'NONE', #15415, #5773 ) ;
#11515 = CARTESIAN_POINT ( 'NONE',  ( 9.657523855033129090E-15, 48.50000000000000000, 52.57311121191334990 ) ) ;
#11516 = CARTESIAN_POINT ( 'NONE',  ( 9.657523855033129090E-15, 28.28125000068279249, 52.57311121191334990 ) ) ;
#11517 = CARTESIAN_POINT ( 'NONE',  ( -40.45084971874737789, 35.58125000068279320, -29.38926261462365730 ) ) ;
#11518 = CARTESIAN_POINT ( 'NONE',  ( -15.40903463028481646, 33.52187500034140299, -47.42413220539093999 ) ) ;
#11519 = VECTOR ( 'NONE', #7312, 1000.000000000000000 ) ;
#11520 = ORIENTED_EDGE ( 'NONE', *, *, #159, .T. ) ;
#11521 = ORIENTED_EDGE ( 'NONE', *, *, #12949, .T. ) ;
#11522 = DIRECTION ( 'NONE',  ( 1.000000000000000000, -0.000000000000000000, 1.734723475976807094E-17 ) ) ;
#11523 = CARTESIAN_POINT ( 'NONE',  ( 19.99999999999999645, 307.0000000000000568, 4.625929269271484533E-15 ) ) ;
#11524 = DIRECTION ( 'NONE',  ( -0.7071067811865451302, 0.000000000000000000, -0.7071067811865500152 ) ) ;
#11525 = CARTESIAN_POINT ( 'NONE',  ( -40.34137639590981905, 49.72187500034139873, -29.30972558990011478 ) ) ;
#11526 = CARTESIAN_POINT ( 'NONE',  ( -49.86468353124999453, 31.75937500034140015, -16.20201782572375393 ) ) ;
#11527 =( LENGTH_UNIT ( ) NAMED_UNIT ( * ) SI_UNIT ( .MILLI., .METRE. ) );
#11528 = AXIS2_PLACEMENT_3D ( 'NONE', #3973, #9215, #130 ) ;
#11529 = CARTESIAN_POINT ( 'NONE',  ( -30.81806926056962226, 48.22187500034139163, 42.41743335407647209 ) ) ;
#11530 = DIRECTION ( 'NONE',  ( 0.000000000000000000, 0.000000000000000000, -1.000000000000000000 ) ) ;
#11531 = CARTESIAN_POINT ( 'NONE',  ( 0.000000000000000000, 20.00000000000000355, 0.000000000000000000 ) ) ;
#11532 = CARTESIAN_POINT ( 'NONE',  ( 15.45084971874736723, 29.18125000068279817, -47.55282581475768211 ) ) ;
#11533 = ORIENTED_EDGE ( 'NONE', *, *, #11691, .T. ) ;
#11534 = CARTESIAN_POINT ( 'NONE',  ( -49.86468353125000164, 47.92187500034139447, 0.000000000000000000 ) ) ;
#11535 = EDGE_CURVE ( 'NONE', #2312, #10158, #11651, .T. ) ;
#11536 = ORIENTED_EDGE ( 'NONE', *, *, #1434, .F. ) ;
#11537 = CARTESIAN_POINT ( 'NONE',  ( -0.4999999999999998890, 38.99242250247064590, 102.0000000000000142 ) ) ;
#11538 = ORIENTED_EDGE ( 'NONE', *, *, #11616, .F. ) ;
#11539 = ORIENTED_EDGE ( 'NONE', *, *, #14467, .F. ) ;
#11540 = CYLINDRICAL_SURFACE ( 'NONE', #1202, 40.00000000000000000 ) ;
#11541 = DIRECTION ( 'NONE',  ( -0.000000000000000000, 0.000000000000000000, -1.000000000000000000 ) ) ;
#11542 = CARTESIAN_POINT ( 'NONE',  ( -30.90169943749473447, 28.29999999999999716, 42.53254041760200721 ) ) ;
#11543 = DIRECTION ( 'NONE',  ( -1.000000000000000000, 0.000000000000000000, 0.000000000000000000 ) ) ;
#11544 = CARTESIAN_POINT ( 'NONE',  ( -30.81806926056962226, 48.15937500034139873, 42.41743335407647919 ) ) ;
#11545 = CARTESIAN_POINT ( 'NONE',  ( 17.28626291527409720, 25.00000000000000355, 18.64048258526027269 ) ) ;
#11546 = CARTESIAN_POINT ( 'NONE',  ( 40.45084971874737079, 26.98125000068279888, -29.38926261462366440 ) ) ;
#11547 = DIRECTION ( 'NONE',  ( 0.000000000000000000, -1.000000000000000000, 0.000000000000000000 ) ) ;
#11548 = FILL_AREA_STYLE_COLOUR ( '', #4135 ) ;
#11549 = CARTESIAN_POINT ( 'NONE',  ( -2.500000000000000000, 242.0000000000000284, 47.99999999999999289 ) ) ;
#11550 = CARTESIAN_POINT ( 'NONE',  ( 30.90169943749475578, 38.48125000068279178, 42.53254041760200010 ) ) ;
#11551 = CARTESIAN_POINT ( 'NONE',  ( -16.79120288457607657, 27.43006142852237517, 101.0000000000000000 ) ) ;
#11552 = VECTOR ( 'NONE', #11690, 1000.000000000000000 ) ;
#11553 = CARTESIAN_POINT ( 'NONE',  ( 40.45084971874737789, 20.80000000000000426, 29.38926261462365375 ) ) ;
#11554 = FILL_AREA_STYLE ('',( #10401 ) ) ;
#11555 = VERTEX_POINT ( 'NONE', #5275 ) ;
#11556 =( BOUNDED_CURVE ( )  B_SPLINE_CURVE ( 2, ( #14416, #14498, #15505, #10777, #4131, #6804, #9206, #5561, #8108, #5709, #15843, #2883, #369 ),
 .UNSPECIFIED., .F., .T. ) 
 B_SPLINE_CURVE_WITH_KNOTS ( ( 3, 2, 2, 2, 2, 2, 3 ),
 ( 0.6166666666666666963, 0.6199999999999999956, 0.6266666666666667052, 0.6333333333333333037, 0.6400000000000000133, 0.6466666666666666119, 0.6500000000000000222 ),
 .UNSPECIFIED. ) 
 CURVE ( )  GEOMETRIC_REPRESENTATION_ITEM ( )  RATIONAL_B_SPLINE_CURVE ( ( 0.9755282581475768211, 0.9755282581475771542, 1.000000000000000000, 0.9510565162951535312, 1.000000000000000000, 0.9510565162951535312, 1.000000000000000000, 0.9510565162951535312, 1.000000000000000000, 0.9510565162951535312, 1.000000000000000000, 0.9755282581475763770, 0.9755282581475768211 ) ) 
 REPRESENTATION_ITEM ( '' )  );
#11557 = CARTESIAN_POINT ( 'NONE',  ( 49.86468353124999453, 38.95937500034139589, -16.20201782572376459 ) ) ;
#11558 = ORIENTED_EDGE ( 'NONE', *, *, #15323, .F. ) ;
#11559 = CARTESIAN_POINT ( 'NONE',  ( -2.518620260143805467, 29.98137973985617677, 40.00000000000000711 ) ) ;
#11560 = DIRECTION ( 'NONE',  ( 1.000000000000000000, 0.000000000000000000, 0.000000000000000000 ) ) ;
#11561 = CARTESIAN_POINT ( 'NONE',  ( 9.631387414534489405E-15, 30.35937500034139447, 52.43083105670540789 ) ) ;
#11562 = VECTOR ( 'NONE', #3243, 1000.000000000000114 ) ;
#11563 = ORIENTED_EDGE ( 'NONE', *, *, #3555, .F. ) ;
#11564 = PRODUCT_DEFINITION_SHAPE ( 'NONE', 'NONE',  #16470 ) ;
#11565 = CARTESIAN_POINT ( 'NONE',  ( 15.45084971874737789, 32.60000000000000142, 47.55282581475767500 ) ) ;
#11566 = CARTESIAN_POINT ( 'NONE',  ( -5.000000000000000000, 102.0000000000000142, 7.580410092413950807 ) ) ;
#11567 = CARTESIAN_POINT ( 'NONE',  ( 46.79661121261624146, 25.00000000000000711, -17.22183559214831661 ) ) ;
#11568 = CARTESIAN_POINT ( 'NONE',  ( -15.40903463028481646, 31.52187500034139944, -47.42413220539093999 ) ) ;
#11569 = EDGE_CURVE ( 'NONE', #6385, #1639, #7665, .T. ) ;
#11570 = CARTESIAN_POINT ( 'NONE',  ( 0.000000000000000000, 52.00000000000000711, -60.00000000000000711 ) ) ;
#11571 = CIRCLE ( 'NONE', #140, 45.00000000000000000 ) ;
#11572 = CARTESIAN_POINT ( 'NONE',  ( 9.631387414534489405E-15, 24.35937500034139447, 52.43083105670540789 ) ) ;
#11573 = CARTESIAN_POINT ( 'NONE',  ( 0.000000000000000000, 22.50000000000000000, 80.00000000000000000 ) ) ;
#11574 = CARTESIAN_POINT ( 'NONE',  ( -49.86468353125000164, 29.92187500034139802, 0.000000000000000000 ) ) ;
#11575 = CARTESIAN_POINT ( 'NONE',  ( 17.50000000000000000, 22.50000000000000355, 101.0000000000000000 ) ) ;
#11576 = CIRCLE ( 'NONE', #16097, 17.50000000000000000 ) ;
#11577 = CARTESIAN_POINT ( 'NONE',  ( 40.45084971874737079, 33.20000000000000284, -29.38926261462366440 ) ) ;
#11578 = CARTESIAN_POINT ( 'NONE',  ( 15.40903463028481113, 33.25937500034140015, -47.42413220539094709 ) ) ;
#11579 = CIRCLE ( 'NONE', #6274, 89.78914894885470233 ) ;
#11580 = CARTESIAN_POINT ( 'NONE',  ( -49.86468353124999453, 29.82187500034139660, -16.20201782572375393 ) ) ;
#11581 = AXIS2_PLACEMENT_3D ( 'NONE', #10620, #7426, #1167 ) ;
#11582 = VECTOR ( 'NONE', #15813, 1000.000000000000227 ) ;
#11583 = AXIS2_PLACEMENT_3D ( 'NONE', #15508, #14265, #2887 ) ;
#11584 = ORIENTED_EDGE ( 'NONE', *, *, #199, .T. ) ;
#11585 = STYLED_ITEM ( 'NONE', ( #8298 ), #1259 ) ;
#11586 = CARTESIAN_POINT ( 'NONE',  ( -40.34137639590981905, 33.65937500034139873, -29.30972558990011478 ) ) ;
#11587 = ORIENTED_EDGE ( 'NONE', *, *, #14133, .T. ) ;
#11588 = VERTEX_POINT ( 'NONE', #170 ) ;
#11589 = EDGE_CURVE ( 'NONE', #3858, #1326, #12735, .T. ) ;
#11590 = PRODUCT_RELATED_PRODUCT_CATEGORY ( 'part', '', ( #7717 ) ) ;
#11591 = CARTESIAN_POINT ( 'NONE',  ( 22.04892374372133546, 283.9500510408986429, -8.524461871865314677 ) ) ;
#11592 = CARTESIAN_POINT ( 'NONE',  ( 15.40903463028482356, 48.45937500034140299, 47.42413220539093999 ) ) ;
#11593 = DIRECTION ( 'NONE',  ( -0.000000000000000000, 1.000000000000000000, -0.000000000000000000 ) ) ;
#11594 = AXIS2_PLACEMENT_3D ( 'NONE', #10433, #11998, #4206 ) ;
#11595 = VECTOR ( 'NONE', #13210, 1000.000000000000000 ) ;
#11596 = CARTESIAN_POINT ( 'NONE',  ( 9.631387414534489405E-15, 24.42187500034139447, 52.43083105670540789 ) ) ;
#11597 = CARTESIAN_POINT ( 'NONE',  ( -3.009228475883398257, 5.937825933686429636, 101.6666710451724214 ) ) ;
#11598 = EDGE_CURVE ( 'NONE', #14169, #532, #2499, .T. ) ;
#11599 = CARTESIAN_POINT ( 'NONE',  ( 9.631387414534489405E-15, 38.42187500034139447, 52.43083105670540789 ) ) ;
#11600 = CARTESIAN_POINT ( 'NONE',  ( 30.81806926056964002, 44.55937500034139020, 42.41743335407646498 ) ) ;
#11601 = LINE ( 'NONE', #32, #15311 ) ;
#11602 = CARTESIAN_POINT ( 'NONE',  ( -30.90169943749473802, 46.30000000000000426, 42.53254041760200721 ) ) ;
#11603 = CARTESIAN_POINT ( 'NONE',  ( 15.45084971874737789, 20.38125000068279746, 47.55282581475767500 ) ) ;
#11604 = CARTESIAN_POINT ( 'NONE',  ( 30.27664397204019409, 40.00000000000000711, -26.14048258526078072 ) ) ;
#11605 = ADVANCED_FACE ( 'NONE', ( #4084 ), #11481, .F. ) ;
#11606 = CARTESIAN_POINT ( 'NONE',  ( -3.210462471511496205E-15, 27.42187500034139092, -52.43083105670540789 ) ) ;
#11607 = AXIS2_PLACEMENT_3D ( 'NONE', #8985, #2660, #4168 ) ;
#11608 = AXIS2_PLACEMENT_3D ( 'NONE', #11679, #15333, #11439 ) ;
#11609 = CIRCLE ( 'NONE', #6860, 17.50000000000000000 ) ;
#11610 = CARTESIAN_POINT ( 'NONE',  ( -7.919222016226816763, 27.55125428154684641, -49.99999999999999289 ) ) ;
#11611 = ORIENTED_EDGE ( 'NONE', *, *, #13150, .F. ) ;
#11612 = CARTESIAN_POINT ( 'NONE',  ( -30.90169943749473802, 36.08125000068280031, 42.53254041760200721 ) ) ;
#11613 = ORIENTED_EDGE ( 'NONE', *, *, #8476, .T. ) ;
#11614 = CARTESIAN_POINT ( 'NONE',  ( 15.45084971874737789, 48.38125000068280457, 47.55282581475767500 ) ) ;
#11615 = FACE_BOUND ( 'NONE', #16126, .T. ) ;
#11616 = EDGE_CURVE ( 'NONE', #2610, #7285, #15314, .T. ) ;
#11617 = CARTESIAN_POINT ( 'NONE',  ( -3.210462471511496205E-15, 45.42187500034138736, -52.43083105670540789 ) ) ;
#11618 = CARTESIAN_POINT ( 'NONE',  ( 49.86468353124999453, 30.95937500034139944, -16.20201782572376459 ) ) ;
#11619 = DIRECTION ( 'NONE',  ( 0.000000000000000000, 0.000000000000000000, -1.000000000000000000 ) ) ;
#11620 = CARTESIAN_POINT ( 'NONE',  ( -50.00000000000000000, 50.00000000000000000, 0.000000000000000000 ) ) ;
#11621 = CARTESIAN_POINT ( 'NONE',  ( -40.34137639590981195, 46.12187500034139731, 29.30972558990012189 ) ) ;
#11622 = SHAPE_DEFINITION_REPRESENTATION ( #7990, #13496 ) ;
#11623 = CARTESIAN_POINT ( 'NONE',  ( 50.00000000000000711, 34.68125000068279462, 16.24598481164530739 ) ) ;
#11624 = EDGE_CURVE ( 'NONE', #1658, #15026, #7497, .T. ) ;
#11625 = CARTESIAN_POINT ( 'NONE',  ( -40.34137639590981195, 48.12187500034139731, 29.30972558990012189 ) ) ;
#11626 = DIRECTION ( 'NONE',  ( 0.000000000000000000, 0.000000000000000000, -1.000000000000000000 ) ) ;
#11627 = ORIENTED_EDGE ( 'NONE', *, *, #1857, .T. ) ;
#11628 = CARTESIAN_POINT ( 'NONE',  ( 30.81806926056962936, 47.22187500034139873, -42.41743335407647209 ) ) ;
#11629 = VECTOR ( 'NONE', #15681, 1000.000000000000000 ) ;
#11630 = VERTEX_POINT ( 'NONE', #12568 ) ;
#11631 = CARTESIAN_POINT ( 'NONE',  ( -49.99999999999999289, 25.89999999999999858, -16.24598481164531449 ) ) ;
#11632 = ORIENTED_EDGE ( 'NONE', *, *, #10873, .T. ) ;
#11633 = ORIENTED_EDGE ( 'NONE', *, *, #1725, .T. ) ;
#11634 = EDGE_CURVE ( 'NONE', #14317, #3456, #8652, .T. ) ;
#11635 = DIRECTION ( 'NONE',  ( 0.000000000000000000, 0.000000000000000000, 1.000000000000000000 ) ) ;
#11636 = DIRECTION ( 'NONE',  ( -0.9361168066628589024, -0.08189960831908939254, -0.3420201433256691570 ) ) ;
#11637 = DIRECTION ( 'NONE',  ( -0.000000000000000000, 1.000000000000000000, -0.000000000000000000 ) ) ;
#11638 = CARTESIAN_POINT ( 'NONE',  ( -49.99999999999999289, 21.90000000000000568, -16.24598481164531449 ) ) ;
#11639 = CARTESIAN_POINT ( 'NONE',  ( -25.00000000000000355, 287.0000000000000568, 2.500000000000001332 ) ) ;
#11640 = CARTESIAN_POINT ( 'NONE',  ( -7.919222016226816763, 25.33250428222964246, -49.99999999999999289 ) ) ;
#11641 = CARTESIAN_POINT ( 'NONE',  ( 9.366734789577542680E-15, 82.00000000000001421, -2.024759949320127682E-14 ) ) ;
#11642 = CARTESIAN_POINT ( 'NONE',  ( -49.86468353124999453, 22.02187500034139589, 16.20201782572377525 ) ) ;
#11643 = VECTOR ( 'NONE', #11290, 1000.000000000000000 ) ;
#11644 = FACE_OUTER_BOUND ( 'NONE', #2105, .T. ) ;
#11645 = CARTESIAN_POINT ( 'NONE',  ( 49.99999999999999289, 38.88125000068279036, -16.24598481164532160 ) ) ;
#11646 = CARTESIAN_POINT ( 'NONE',  ( -2.445080149700054274E-14, 46.50000000000000711, 50.00000000000000000 ) ) ;
#11647 = CARTESIAN_POINT ( 'NONE',  ( 30.90169943749475578, 20.69999999999999574, 42.53254041760200010 ) ) ;
#11648 = ORIENTED_EDGE ( 'NONE', *, *, #5214, .F. ) ;
#11649 = CARTESIAN_POINT ( 'NONE',  ( -30.81806926056963292, 39.55937500034139731, -42.41743335407647209 ) ) ;
#11650 = VERTEX_POINT ( 'NONE', #11332 ) ;
#11651 = LINE ( 'NONE', #12658, #7370 ) ;
#11652 = CARTESIAN_POINT ( 'NONE',  ( 30.81806926056962936, 29.15937500034139518, -42.41743335407647209 ) ) ;
#11653 = ORIENTED_EDGE ( 'NONE', *, *, #12330, .T. ) ;
#11654 = LINE ( 'NONE', #7825, #6286 ) ;
#11655 = DIRECTION ( 'NONE',  ( 1.000000000000000000, 0.000000000000000000, 0.000000000000000000 ) ) ;
#11656 = LINE ( 'NONE', #7910, #1932 ) ;
#11657 = CARTESIAN_POINT ( 'NONE',  ( -3.210462471511496205E-15, 33.42187500034139447, -52.43083105670540789 ) ) ;
#11658 = DIRECTION ( 'NONE',  ( -0.9135454576426005335, -0.4067366430758011520, 0.000000000000000000 ) ) ;
#11659 = EDGE_CURVE ( 'NONE', #6571, #3157, #10283, .T. ) ;
#11660 = CARTESIAN_POINT ( 'NONE',  ( 30.81806926056962936, 21.15937500034139518, -42.41743335407646498 ) ) ;
#11661 = CARTESIAN_POINT ( 'NONE',  ( -47.39803307437431101, 19.99999999999999645, 15.49002591438328302 ) ) ;
#11662 = CARTESIAN_POINT ( 'NONE',  ( 49.86468353124999453, 29.02187500034139234, -16.20201782572376104 ) ) ;
#11663 =( BOUNDED_CURVE ( )  B_SPLINE_CURVE ( 2, ( #975, #15948, #7395, #6074, #8303, #16200, #13369, #13694, #1055, #16027, #14685, #8469, #14939 ),
 .UNSPECIFIED., .F., .T. ) 
 B_SPLINE_CURVE_WITH_KNOTS ( ( 3, 2, 2, 2, 2, 2, 3 ),
 ( 0.2833333333333333814, 0.2866666666666666807, 0.2933333333333333348, 0.2999999999999999889, 0.3066666666666666430, 0.3133333333333333526, 0.3166666666666667074 ),
 .UNSPECIFIED. ) 
 CURVE ( )  GEOMETRIC_REPRESENTATION_ITEM ( )  RATIONAL_B_SPLINE_CURVE ( ( 0.9755282581475768211, 0.9755282581475770431, 1.000000000000000000, 0.9510565162951535312, 1.000000000000000000, 0.9510565162951535312, 1.000000000000000000, 0.9510565162951535312, 1.000000000000000000, 0.9510565162951535312, 1.000000000000000000, 0.9755282581475765991, 0.9755282581475768211 ) ) 
 REPRESENTATION_ITEM ( '' )  );
#11664 = FACE_OUTER_BOUND ( 'NONE', #11220, .T. ) ;
#11665 = CARTESIAN_POINT ( 'NONE',  ( -30.90169943749474868, 33.69999999999998863, -42.53254041760200721 ) ) ;
#11666 = CARTESIAN_POINT ( 'NONE',  ( 49.86468353125000164, 34.85937500034140157, -6.106662507704105588E-15 ) ) ;
#11667 = CARTESIAN_POINT ( 'NONE',  ( 49.86468353125000164, 30.92187500034139802, -6.106662507704105588E-15 ) ) ;
#11668 = VERTEX_POINT ( 'NONE', #10325 ) ;
#11669 = CARTESIAN_POINT ( 'NONE',  ( -30.81806926056963292, 33.55937500034139020, -42.41743335407646498 ) ) ;
#11670 = ORIENTED_EDGE ( 'NONE', *, *, #7141, .T. ) ;
#11671 = CARTESIAN_POINT ( 'NONE',  ( 30.00000000000000711, 282.0000000000000000, -12.50000000000000178 ) ) ;
#11672 = CARTESIAN_POINT ( 'NONE',  ( -40.34137639590981195, 48.05937500034139731, 29.30972558990012189 ) ) ;
#11673 = AXIS2_PLACEMENT_3D ( 'NONE', #12534, #5075, #9042 ) ;
#11674 = CARTESIAN_POINT ( 'NONE',  ( 5.510910596163089556E-15, 262.0000000000000000, -45.00000000000000000 ) ) ;
#11675 = CARTESIAN_POINT ( 'NONE',  ( 26.02446187186531645, 283.9500510408985861, 4.548923743721332791 ) ) ;
#11676 = CARTESIAN_POINT ( 'NONE',  ( -26.95005104082770231, 283.0244618719127629, 6.400102081653812114 ) ) ;
#11677 = CARTESIAN_POINT ( 'NONE',  ( -49.86468353124999453, 34.02187500034140299, 16.20201782572377525 ) ) ;
#11678 = CARTESIAN_POINT ( 'NONE',  ( -30.81806926056962226, 44.15937500034139163, 42.41743335407647209 ) ) ;
#11679 = CARTESIAN_POINT ( 'NONE',  ( 0.000000000000000000, 55.00000000000000711, 0.000000000000000000 ) ) ;
#11680 = CARTESIAN_POINT ( 'NONE',  ( 15.45084971874737789, 38.60000000000000142, 47.55282581475767500 ) ) ;
#11681 = CARTESIAN_POINT ( 'NONE',  ( 50.00000000000000000, 20.78125000068279959, -6.123233995736766085E-15 ) ) ;
#11682 = EDGE_CURVE ( 'NONE', #2031, #13278, #10550, .T. ) ;
#11683 = CARTESIAN_POINT ( 'NONE',  ( -7.919222016226816763, 35.33250428222964246, -49.99999999999999289 ) ) ;
#11684 = CARTESIAN_POINT ( 'NONE',  ( 49.86468353124999453, 27.02187500034139589, -16.20201782572376459 ) ) ;
#11685 = DIRECTION ( 'NONE',  ( 0.000000000000000000, 1.000000000000000000, 0.000000000000000000 ) ) ;
#11686 = ORIENTED_EDGE ( 'NONE', *, *, #15377, .F. ) ;
#11687 = CARTESIAN_POINT ( 'NONE',  ( 40.45084971874737789, 34.58125000068280031, 29.38926261462365375 ) ) ;
#11688 = ORIENTED_EDGE ( 'NONE', *, *, #6754, .T. ) ;
#11689 = CARTESIAN_POINT ( 'NONE',  ( -38.60409515610530917, 20.00000000000000355, 31.77615201968871617 ) ) ;
#11690 = DIRECTION ( 'NONE',  ( -0.000000000000000000, -0.000000000000000000, 1.000000000000000000 ) ) ;
#11691 = EDGE_CURVE ( 'NONE', #8272, #3201, #7097, .T. ) ;
#11692 = CARTESIAN_POINT ( 'NONE',  ( -3.111920190527341144E-15, 29.28125000068279604, -50.00000000000000000 ) ) ;
#11693 = CARTESIAN_POINT ( 'NONE',  ( 3.505380114644272460, 100.5662537783984192, -8.566253778398381868 ) ) ;
#11694 = CARTESIAN_POINT ( 'NONE',  ( 9.631387414534489405E-15, 22.35937500034139802, 52.43083105670540789 ) ) ;
#11695 = CARTESIAN_POINT ( 'NONE',  ( 7.977241335952203194, 17.31698729810786475, 101.0000000000000000 ) ) ;
#11696 = CARTESIAN_POINT ( 'NONE',  ( 9.631387414534489405E-15, 42.42187500034140157, 52.43083105670540789 ) ) ;
#11697 = EDGE_CURVE ( 'NONE', #13297, #7881, #9491, .T. ) ;
#11698 = CARTESIAN_POINT ( 'NONE',  ( 0.000000000000000000, 262.0000000000000000, -40.00000000000000000 ) ) ;
#11699 = EDGE_CURVE ( 'NONE', #2224, #12941, #14376, .T. ) ;
#11700 = CARTESIAN_POINT ( 'NONE',  ( -15.40903463028481646, 47.52187500034139589, -47.42413220539093999 ) ) ;
#11701 = DIRECTION ( 'NONE',  ( 1.000000000000000000, 0.000000000000000000, 0.000000000000000000 ) ) ;
#11702 = VERTEX_POINT ( 'NONE', #1824 ) ;
#11703 = EDGE_CURVE ( 'NONE', #9620, #2516, #15838, .T. ) ;
#11704 = CARTESIAN_POINT ( 'NONE',  ( -40.34137639590981195, 46.12187500034139731, 29.30972558990012189 ) ) ;
#11705 = ORIENTED_EDGE ( 'NONE', *, *, #8894, .F. ) ;
#11706 = FACE_OUTER_BOUND ( 'NONE', #9871, .T. ) ;
#11707 = EDGE_LOOP ( 'NONE', ( #12999, #11748, #6882, #1702 ) ) ;
#11708 = ORIENTED_EDGE ( 'NONE', *, *, #2037, .F. ) ;
#11709 = VECTOR ( 'NONE', #9654, 1000.000000000000000 ) ;
#11710 = DIRECTION ( 'NONE',  ( 0.000000000000000000, -1.000000000000000000, 0.000000000000000000 ) ) ;
#11711 = CARTESIAN_POINT ( 'NONE',  ( -1.240322475938754499E-13, 38.28125000068280315, 50.00000000000000000 ) ) ;
#11712 = CARTESIAN_POINT ( 'NONE',  ( -50.00000000000000000, 24.00000000000000000, 0.000000000000000000 ) ) ;
#11713 = CARTESIAN_POINT ( 'NONE',  ( 9.631387414534489405E-15, 42.35937500034140157, 52.43083105670540789 ) ) ;
#11714 = CARTESIAN_POINT ( 'NONE',  ( -49.99999999999999289, 25.88125000068279746, 16.24598481164533226 ) ) ;
#11715 = DIRECTION ( 'NONE',  ( -0.000000000000000000, 1.000000000000000000, -0.000000000000000000 ) ) ;
#11716 = CARTESIAN_POINT ( 'NONE',  ( -40.34137639590981195, 26.12187500034139731, 29.30972558990012189 ) ) ;
#11717 =( NAMED_UNIT ( * ) PLANE_ANGLE_UNIT ( ) SI_UNIT ( $, .RADIAN. ) );
#11718 = DIRECTION ( 'NONE',  ( 0.000000000000000000, 1.000000000000000000, 0.000000000000000000 ) ) ;
#11719 = CARTESIAN_POINT ( 'NONE',  ( 15.45084971874737789, 42.38125000068279746, 47.55282581475767500 ) ) ;
#11720 = FACE_OUTER_BOUND ( 'NONE', #15077, .T. ) ;
#11721 = CARTESIAN_POINT ( 'NONE',  ( 7.919222016226693306, 20.33250428222963890, 50.00000000000003553 ) ) ;
#11722 = ADVANCED_FACE ( 'NONE', ( #3164 ), #9155, .F. ) ;
#11723 = ORIENTED_EDGE ( 'NONE', *, *, #15738, .T. ) ;
#11724 = CARTESIAN_POINT ( 'NONE',  ( -15.40903463028481646, 35.45937500034139589, -47.42413220539093999 ) ) ;
#11725 = ORIENTED_EDGE ( 'NONE', *, *, #15831, .F. ) ;
#11726 = EDGE_CURVE ( 'NONE', #1499, #1769, #7987, .T. ) ;
#11727 = CARTESIAN_POINT ( 'NONE',  ( -30.90169943749473802, 48.08125000068278609, 42.53254041760200721 ) ) ;
#11728 = CARTESIAN_POINT ( 'NONE',  ( 0.000000000000000000, 20.00000000000000355, 0.000000000000000000 ) ) ;
#11729 = CARTESIAN_POINT ( 'NONE',  ( 15.40903463028482356, 20.45937500034139589, 47.42413220539093999 ) ) ;
#11730 = EDGE_LOOP ( 'NONE', ( #13058, #189, #1685, #6398 ) ) ;
#11731 = DIRECTION ( 'NONE',  ( 0.000000000000000000, -1.000000000000000000, 0.000000000000000000 ) ) ;
#11732 = DIRECTION ( 'NONE',  ( 0.000000000000000000, -0.000000000000000000, 1.000000000000000000 ) ) ;
#11733 = CARTESIAN_POINT ( 'NONE',  ( 1.875620865444973696E-15, 37.00000000000001421, -3.248670634687016947E-15 ) ) ;
#11734 = CARTESIAN_POINT ( 'NONE',  ( 40.34137639590981905, 28.72187500034139873, 29.30972558990010768 ) ) ;
#11735 = DIRECTION ( 'NONE',  ( 0.000000000000000000, 0.000000000000000000, 1.000000000000000000 ) ) ;
#11736 = CARTESIAN_POINT ( 'NONE',  ( 2.313956153764268553, 5.143932793412055560, 99.06765316570249524 ) ) ;
#11737 = DIRECTION ( 'NONE',  ( 5.069245582283711292E-17, 1.000000000000000000, -8.780190904559503697E-17 ) ) ;
#11738 = CARTESIAN_POINT ( 'NONE',  ( 30.81806926056964002, 26.62187500034139731, 42.41743335407646498 ) ) ;
#11739 = CARTESIAN_POINT ( 'NONE',  ( 7.977241335952203194, 17.31698729810786475, 102.0000000000000142 ) ) ;
#11740 = CARTESIAN_POINT ( 'NONE',  ( 50.00000000000000711, 36.89999999999999858, 16.24598481164530739 ) ) ;
#11741 = CARTESIAN_POINT ( 'NONE',  ( -49.86468353125000164, 31.85937500034139447, 0.000000000000000000 ) ) ;
#11742 = CARTESIAN_POINT ( 'NONE',  ( 19.99999999999999289, 312.0000000000000568, 7.500000000000002665 ) ) ;
#11743 = ORIENTED_EDGE ( 'NONE', *, *, #11109, .T. ) ;
#11744 = EDGE_CURVE ( 'NONE', #7461, #9095, #6919, .T. ) ;
#11745 = AXIS2_PLACEMENT_3D ( 'NONE', #9374, #14586, #621 ) ;
#11746 = CARTESIAN_POINT ( 'NONE',  ( 15.40903463028481113, 31.25937500034140015, -47.42413220539094709 ) ) ;
#11747 = EDGE_CURVE ( 'NONE', #4841, #6384, #15791, .T. ) ;
#11748 = ORIENTED_EDGE ( 'NONE', *, *, #3464, .F. ) ;
#11749 = DIRECTION ( 'NONE',  ( 0.000000000000000000, 0.000000000000000000, 1.000000000000000000 ) ) ;
#11750 = CARTESIAN_POINT ( 'NONE',  ( -15.40903463028480580, 40.25937500034139305, 47.42413220539094709 ) ) ;
#11751 = DIRECTION ( 'NONE',  ( -0.2079116908177532641, -0.9781476007338069101, 0.000000000000000000 ) ) ;
#11752 = CARTESIAN_POINT ( 'NONE',  ( 25.25536947722714842, 285.3889217077638705, 3.010738954466165129 ) ) ;
#11753 = CARTESIAN_POINT ( 'NONE',  ( -25.56848793686307175, 282.5058351977235134, 10.28424396843205635 ) ) ;
#11754 = CARTESIAN_POINT ( 'NONE',  ( 15.40903463028481113, 33.32187500034139305, -47.42413220539094709 ) ) ;
#11755 = CARTESIAN_POINT ( 'NONE',  ( 40.34137639590981905, 36.65937500034139873, 29.30972558990010768 ) ) ;
#11756 = DIRECTION ( 'NONE',  ( 0.000000000000000000, 1.000000000000000000, 0.000000000000000000 ) ) ;
#11757 = CARTESIAN_POINT ( 'NONE',  ( 15.45084971874737789, 42.60000000000000142, 47.55282581475767500 ) ) ;
#11758 = CIRCLE ( 'NONE', #8838, 17.50000000000000000 ) ;
#11759 = ADVANCED_BREP_SHAPE_REPRESENTATION ( '', ( #3636, #15812 ), #10512 ) ;
#11760 = CARTESIAN_POINT ( 'NONE',  ( 49.86468353124999453, 48.95937500034140299, -16.20201782572376459 ) ) ;
#11761 = CARTESIAN_POINT ( 'NONE',  ( 49.86468353125001585, 44.82187500034138594, 16.20201782572375038 ) ) ;
#11762 = CARTESIAN_POINT ( 'NONE',  ( 49.86468353125001585, 26.82187500034138949, 16.20201782572375038 ) ) ;
#11763 = CARTESIAN_POINT ( 'NONE',  ( -3.210462471511496205E-15, 49.35937500034138736, -52.43083105670540789 ) ) ;
#11764 = VERTEX_POINT ( 'NONE', #1586 ) ;
#11765 = CARTESIAN_POINT ( 'NONE',  ( -30.90169943749473802, 34.08125000068279320, 42.53254041760200721 ) ) ;
#11766 = ORIENTED_EDGE ( 'NONE', *, *, #9514, .T. ) ;
#11767 = CARTESIAN_POINT ( 'NONE',  ( 40.45084971874737079, 48.98125000068279888, -29.38926261462366440 ) ) ;
#11768 = CARTESIAN_POINT ( 'NONE',  ( 9.189545401991395579, 24.96013318841451678, 101.0000000000000000 ) ) ;
#11769 = CARTESIAN_POINT ( 'NONE',  ( 4.320770838041294581, 30.97531352606685218, 101.0000000000000000 ) ) ;
#11770 = CARTESIAN_POINT ( 'NONE',  ( 30.81806926056964002, 48.62187500034139731, 42.41743335407646498 ) ) ;
#11771 = CARTESIAN_POINT ( 'NONE',  ( -49.86468353125000164, 23.85937500034139447, 0.000000000000000000 ) ) ;
#11772 = CARTESIAN_POINT ( 'NONE',  ( 30.81806926056964002, 42.62187500034139731, 42.41743335407646498 ) ) ;
#11773 =( NAMED_UNIT ( * ) PLANE_ANGLE_UNIT ( ) SI_UNIT ( $, .RADIAN. ) );
#11774 = DIRECTION ( 'NONE',  ( 0.000000000000000000, 0.000000000000000000, -1.000000000000000000 ) ) ;
#11775 = AXIS2_PLACEMENT_3D ( 'NONE', #990, #13382, #4510 ) ;
#11776 = CARTESIAN_POINT ( 'NONE',  ( -40.34137639590981905, 49.72187500034139873, -29.30972558990011478 ) ) ;
#11777 = DIRECTION ( 'NONE',  ( 1.156482317317871478E-16, 0.000000000000000000, 1.000000000000000000 ) ) ;
#11778 = VERTEX_POINT ( 'NONE', #569 ) ;
#11779 = ADVANCED_FACE ( 'NONE', ( #1899 ), #9403, .F. ) ;
#11780 = CARTESIAN_POINT ( 'NONE',  ( -49.86468353124999453, 19.95937500034138878, 16.20201782572377525 ) ) ;
#11781 = EDGE_LOOP ( 'NONE', ( #13466, #8629, #13827, #2643 ) ) ;
#11782 = CARTESIAN_POINT ( 'NONE',  ( 9.332040320058006538E-15, 92.00000000000001421, -14.08089297201393109 ) ) ;
#11783 = ORIENTED_EDGE ( 'NONE', *, *, #8705, .F. ) ;
#11784 = ORIENTED_EDGE ( 'NONE', *, *, #6634, .T. ) ;
#11785 = CARTESIAN_POINT ( 'NONE',  ( 6.123233995736766085E-15, 20.00000000000000355, -50.00000000000000000 ) ) ;
#11786 = DIRECTION ( 'NONE',  ( -0.000000000000000000, 1.000000000000000000, -0.000000000000000000 ) ) ;
#11787 = EDGE_CURVE ( 'NONE', #10200, #10702, #10731, .T. ) ;
#11788 = AXIS2_PLACEMENT_3D ( 'NONE', #4567, #10808, #14857 ) ;
#11789 = DIRECTION ( 'NONE',  ( 0.000000000000000000, -0.9848077530122080203, 0.1736481776669307198 ) ) ;
#11790 = CARTESIAN_POINT ( 'NONE',  ( -49.99999999999999289, 23.90000000000000213, -16.24598481164531449 ) ) ;
#11791 = CARTESIAN_POINT ( 'NONE',  ( 40.34137639590981195, 45.05937500034139731, -29.30972558990011834 ) ) ;
#11792 = FACE_OUTER_BOUND ( 'NONE', #4236, .T. ) ;
#11793 = LINE ( 'NONE', #15619, #13512 ) ;
#11794 = CARTESIAN_POINT ( 'NONE',  ( -49.99999999999999289, 33.68125000068278752, -16.24598481164531449 ) ) ;
#11795 = EDGE_CURVE ( 'NONE', #15183, #13541, #13982, .T. ) ;
#11796 = FACE_OUTER_BOUND ( 'NONE', #9867, .T. ) ;
#11797 = CARTESIAN_POINT ( 'NONE',  ( 15.45084971874737789, 40.38125000068280457, 47.55282581475767500 ) ) ;
#11798 =( BOUNDED_CURVE ( )  B_SPLINE_CURVE ( 2, ( #8823, #13886, #2501, #7581, #7746, #7668, #12738, #6426, #14056, #2672, #11565, #12814, #1416 ),
 .UNSPECIFIED., .F., .F. ) 
 B_SPLINE_CURVE_WITH_KNOTS ( ( 3, 2, 2, 2, 2, 2, 3 ),
 ( 0.5500000000000000444, 0.5533333333333333437, 0.5600000000000000533, 0.5666666666666666519, 0.5733333333333333615, 0.5799999999999999600, 0.5833333333333333703 ),
 .UNSPECIFIED. ) 
 CURVE ( )  GEOMETRIC_REPRESENTATION_ITEM ( )  RATIONAL_B_SPLINE_CURVE ( ( 0.9755282581475768211, 0.9755282581475771542, 1.000000000000000000, 0.9510565162951535312, 1.000000000000000000, 0.9510565162951535312, 1.000000000000000000, 0.9510565162951535312, 1.000000000000000000, 0.9510565162951535312, 1.000000000000000000, 0.9755282581475763770, 0.9755282581475768211 ) ) 
 REPRESENTATION_ITEM ( '' )  );
#11799 = CARTESIAN_POINT ( 'NONE',  ( -2.464234863135557063, 13.31155363843772932, 101.0000000000000000 ) ) ;
#11800 = DIRECTION ( 'NONE',  ( 1.003171929053523391E-16, -0.5735764363510476027, 0.8191520442889907994 ) ) ;
#11801 = ORIENTED_EDGE ( 'NONE', *, *, #9141, .T. ) ;
#11802 = CIRCLE ( 'NONE', #10481, 16.50000000000000711 ) ;
#11803 = EDGE_CURVE ( 'NONE', #2563, #12657, #7361, .T. ) ;
#11804 = CARTESIAN_POINT ( 'NONE',  ( 40.34137639590981905, 38.65937500034139873, 29.30972558990010768 ) ) ;
#11805 = ORIENTED_EDGE ( 'NONE', *, *, #9780, .F. ) ;
#11806 = ORIENTED_EDGE ( 'NONE', *, *, #15452, .F. ) ;
#11807 = CARTESIAN_POINT ( 'NONE',  ( 15.45084971874736723, 49.18125000068279462, -47.55282581475768211 ) ) ;
#11808 = DIRECTION ( 'NONE',  ( 0.000000000000000000, 0.000000000000000000, -1.000000000000000000 ) ) ;
#11809 = CARTESIAN_POINT ( 'NONE',  ( -40.34137639590981905, 23.65937500034139518, -29.30972558990011478 ) ) ;
#11810 = ORIENTED_EDGE ( 'NONE', *, *, #3877, .T. ) ;
#11811 = PLANE ( 'NONE',  #13171 ) ;
#11812 = DIRECTION ( 'NONE',  ( 0.7431448254773955764, -0.6691306063588567943, 0.000000000000000000 ) ) ;
#11813 = DIRECTION ( 'NONE',  ( 1.000000000000000000, -7.137148015447435579E-15, 0.000000000000000000 ) ) ;
#11814 = CARTESIAN_POINT ( 'NONE',  ( 9.631387414534489405E-15, 30.42187500034139447, 52.43083105670540789 ) ) ;
#11815 = CARTESIAN_POINT ( 'NONE',  ( -7.919222016226934890, 30.22999571913595318, 49.99999999999996447 ) ) ;
#11816 = CARTESIAN_POINT ( 'NONE',  ( -43.10890719796073256, 20.03031439394993996, 25.50054622961014772 ) ) ;
#11817 = CARTESIAN_POINT ( 'NONE',  ( -48.28553921371794644, 20.00000000000000355, 12.45074877219254894 ) ) ;
#11818 = CARTESIAN_POINT ( 'NONE',  ( -15.40903463028480580, 28.32187500034139660, 47.42413220539094709 ) ) ;
#11819 = DIRECTION ( 'NONE',  ( 0.4999999999999919509, 0.8660254037844432595, 0.000000000000000000 ) ) ;
#11820 = CARTESIAN_POINT ( 'NONE',  ( -49.99999999999999289, 36.10000000000000853, 16.24598481164533226 ) ) ;
#11821 = CARTESIAN_POINT ( 'NONE',  ( -30.81806926056962226, 30.15937500034139163, 42.41743335407647919 ) ) ;
#11822 = ADVANCED_FACE ( 'NONE', ( #6992, #1745 ), #10488, .T. ) ;
#11823 = LINE ( 'NONE', #11742, #3800 ) ;
#11824 = ORIENTED_EDGE ( 'NONE', *, *, #5536, .T. ) ;
#11825 = VECTOR ( 'NONE', #9135, 1000.000000000000000 ) ;
#11826 = CARTESIAN_POINT ( 'NONE',  ( 9.631387414534489405E-15, 32.35937500034139447, 52.43083105670540789 ) ) ;
#11827 = ORIENTED_EDGE ( 'NONE', *, *, #125, .T. ) ;
#11828 = CARTESIAN_POINT ( 'NONE',  ( -41.63290517038959848, 96.34995309285439191, -5.000000000000000000 ) ) ;
#11829 = CARTESIAN_POINT ( 'NONE',  ( -49.86468353125000164, 41.85937500034139447, 0.000000000000000000 ) ) ;
#11830 = CARTESIAN_POINT ( 'NONE',  ( -17.34476375915448187, 20.17423772944842142, 101.0000000000000000 ) ) ;
#11831 = CARTESIAN_POINT ( 'NONE',  ( 26.40559293885843317, 283.2826504366940412, 8.905592938859888008 ) ) ;
#11832 = CARTESIAN_POINT ( 'NONE',  ( -25.15991675646742465, 285.7035871579729474, 2.819833512935955078 ) ) ;
#11833 = CARTESIAN_POINT ( 'NONE',  ( 49.86468353124999453, 35.02187500034139589, -16.20201782572376459 ) ) ;
#11834 = CARTESIAN_POINT ( 'NONE',  ( 49.86468353125001585, 36.75937500034139305, 16.20201782572375038 ) ) ;
#11835 = VECTOR ( 'NONE', #3327, 1000.000000000000000 ) ;
#11836 = DIRECTION ( 'NONE',  ( 0.000000000000000000, 0.000000000000000000, 1.000000000000000000 ) ) ;
#11837 = AXIS2_PLACEMENT_3D ( 'NONE', #12571, #7500, #9922 ) ;
#11838 = CARTESIAN_POINT ( 'NONE',  ( -3.219174618344376363E-15, 41.49999999999999289, -52.57311121191334990 ) ) ;
#11839 = PRODUCT_DEFINITION_SHAPE ( 'NONE', 'NONE',  #295 ) ;
#11840 = ADVANCED_FACE ( 'NONE', ( #5748 ), #5429, .F. ) ;
#11841 = CARTESIAN_POINT ( 'NONE',  ( -49.99999999999999289, 19.88125000068279746, 16.24598481164533226 ) ) ;
#11842 =( REPRESENTATION_RELATIONSHIP ('NONE','NONE', #6178, #13393 ) REPRESENTATION_RELATIONSHIP_WITH_TRANSFORMATION ( #8280 )SHAPE_REPRESENTATION_RELATIONSHIP( ) );
#11843 = CARTESIAN_POINT ( 'NONE',  ( 49.86468353124999453, 47.02187500034139589, -16.20201782572376459 ) ) ;
#11844 =( GEOMETRIC_REPRESENTATION_CONTEXT ( 3 ) GLOBAL_UNCERTAINTY_ASSIGNED_CONTEXT ( ( #8253 ) ) GLOBAL_UNIT_ASSIGNED_CONTEXT ( ( #9805, #809, #11046 ) ) REPRESENTATION_CONTEXT ( 'NONE', 'WORKASPACE' ) );
#11845 = CARTESIAN_POINT ( 'NONE',  ( 30.81806926056962936, 27.22187500034139518, -42.41743335407647209 ) ) ;
#11846 = CIRCLE ( 'NONE', #13960, 16.50000000000000711 ) ;
#11847 = CARTESIAN_POINT ( 'NONE',  ( -15.45084971874737256, 27.38125000068280102, -47.55282581475767500 ) ) ;
#11848 = VECTOR ( 'NONE', #4059, 1000.000000000000000 ) ;
#11849 = VERTEX_POINT ( 'NONE', #10578 ) ;
#11850 = VECTOR ( 'NONE', #10247, 1000.000000000000000 ) ;
#11851 = AXIS2_PLACEMENT_3D ( 'NONE', #13548, #11156, #11233 ) ;
#11853 = CARTESIAN_POINT ( 'NONE',  ( -3.219174618344376363E-15, 33.28125000068280315, -52.57311121191334990 ) ) ;
#11852 = VECTOR ( 'NONE', #3518, 999.9999999999998863 ) ;
#11854 = ORIENTED_EDGE ( 'NONE', *, *, #10590, .T. ) ;
#11855 = DIRECTION ( 'NONE',  ( 0.000000000000000000, 0.000000000000000000, 1.000000000000000000 ) ) ;
#11856 = CARTESIAN_POINT ( 'NONE',  ( -2.547328955960238000E-13, 34.28125000068279604, 49.99999999999999289 ) ) ;
#11857 = CARTESIAN_POINT ( 'NONE',  ( 40.34137639590981195, 49.12187500034139731, -29.30972558990011834 ) ) ;
#11858 = CARTESIAN_POINT ( 'NONE',  ( 49.86468353125000164, 26.85937500034139802, -6.106662507704105588E-15 ) ) ;
#11859 = CARTESIAN_POINT ( 'NONE',  ( -30.90169943749473447, 40.08125000068279320, 42.53254041760200721 ) ) ;
#11860 = CARTESIAN_POINT ( 'NONE',  ( 40.34137639590981905, 38.72187500034139873, 29.30972558990010768 ) ) ;
#11861 = AXIS2_PLACEMENT_3D ( 'NONE', #9676, #8580, #7362 ) ;
#11862 = DIRECTION ( 'NONE',  ( 0.000000000000000000, 0.000000000000000000, 1.000000000000000000 ) ) ;
#11863 = VECTOR ( 'NONE', #2779, 1000.000000000000000 ) ;
#11864 = CIRCLE ( 'NONE', #168, 40.00000000000000000 ) ;
#11865 = CARTESIAN_POINT ( 'NONE',  ( 30.81806926056964002, 48.62187500034139731, 42.41743335407647209 ) ) ;
#11866 = ORIENTED_EDGE ( 'NONE', *, *, #15572, .T. ) ;
#11867 = CARTESIAN_POINT ( 'NONE',  ( 49.86468353125001585, 20.75937500034140015, 16.20201782572375038 ) ) ;
#11868 = ORIENTED_EDGE ( 'NONE', *, *, #4641, .T. ) ;
#11869 = ORIENTED_EDGE ( 'NONE', *, *, #10222, .F. ) ;
#11870 = EDGE_CURVE ( 'NONE', #6639, #13132, #5516, .T. ) ;
#11871 = AXIS2_PLACEMENT_3D ( 'NONE', #16026, #11963, #5652 ) ;
#11872 = ADVANCED_FACE ( 'NONE', ( #14299 ), #2921, .T. ) ;
#11873 = PLANE ( 'NONE',  #13995 ) ;
#11874 = CARTESIAN_POINT ( 'NONE',  ( 0.000000000000000000, 252.1309828287255357, 0.000000000000000000 ) ) ;
#11875 = AXIS2_PLACEMENT_3D ( 'NONE', #12360, #6974, #12114 ) ;
#11876 = DIRECTION ( 'NONE',  ( 0.000000000000000000, 0.000000000000000000, -1.000000000000000000 ) ) ;
#11877 = CARTESIAN_POINT ( 'NONE',  ( 15.45084971874736723, 23.40000000000000213, -47.55282581475768211 ) ) ;
#11878 = CARTESIAN_POINT ( 'NONE',  ( 15.40903463028482356, 44.45937500034139589, 47.42413220539093999 ) ) ;
#11879 = CARTESIAN_POINT ( 'NONE',  ( -15.45084971874737256, 31.38125000068280102, -47.55282581475767500 ) ) ;
#11880 = CARTESIAN_POINT ( 'NONE',  ( 0.000000000000000000, 217.0000000000000284, 0.000000000000000000 ) ) ;
#11881 = LINE ( 'NONE', #478, #10804 ) ;
#11882 = CARTESIAN_POINT ( 'NONE',  ( 50.00000000000000711, 48.90000000000000568, 16.24598481164530739 ) ) ;
#11883 = CARTESIAN_POINT ( 'NONE',  ( 30.90169943749475578, 32.48125000068280599, 42.53254041760200010 ) ) ;
#11884 = CARTESIAN_POINT ( 'NONE',  ( 2.500000000000000000, 244.0000000000000284, -47.99999999999999289 ) ) ;
#11885 = CARTESIAN_POINT ( 'NONE',  ( 15.45084971874736723, 23.18125000068279817, -47.55282581475768211 ) ) ;
#11886 = DIRECTION ( 'NONE',  ( 0.7071067811865465735, 0.7071067811865484609, -1.635512977795596615E-16 ) ) ;
#11887 = EDGE_CURVE ( 'NONE', #3182, #10580, #13706, .T. ) ;
#11888 = PRODUCT_DEFINITION ( 'UNKNOWN', '', #8385, #7925 ) ;
#11889 = ORIENTED_EDGE ( 'NONE', *, *, #5900, .F. ) ;
#11890 = CARTESIAN_POINT ( 'NONE',  ( -3.210462471511496205E-15, 37.35937500034139447, -52.43083105670540789 ) ) ;
#11891 = EDGE_LOOP ( 'NONE', ( #8389, #12010, #10426, #9621 ) ) ;
#11892 = ORIENTED_EDGE ( 'NONE', *, *, #13214, .F. ) ;
#11893 = CARTESIAN_POINT ( 'NONE',  ( -40.45084971874737789, 49.58125000068280031, -29.38926261462365730 ) ) ;
#11894 = DIRECTION ( 'NONE',  ( -1.000000000000000000, -1.224646799147353207E-16, 0.000000000000000000 ) ) ;
#11895 = CARTESIAN_POINT ( 'NONE',  ( -49.86468353124999453, 25.75937500034140015, -16.20201782572375393 ) ) ;
#11896 = EDGE_LOOP ( 'NONE', ( #10599, #9072, #16128, #12757 ) ) ;
#11897 = AXIS2_PLACEMENT_3D ( 'NONE', #7470, #1470, #13935 ) ;
#11898 = CARTESIAN_POINT ( 'NONE',  ( -9.500222237632405253, 22.00424054664139817, 102.0000000000000142 ) ) ;
#11899 = CARTESIAN_POINT ( 'NONE',  ( 0.000000000000000000, 102.0000000000000142, 5.000000000000000000 ) ) ;
#11900 = LINE ( 'NONE', #15640, #12286 ) ;
#11901 = CARTESIAN_POINT ( 'NONE',  ( -30.81806926056963292, 29.62187500034139376, -42.41743335407646498 ) ) ;
#11902 =( BOUNDED_CURVE ( )  B_SPLINE_CURVE ( 3, ( #7106, #14413, #12162, #10447 ),
 .UNSPECIFIED., .F., .F. ) 
 B_SPLINE_CURVE_WITH_KNOTS ( ( 4, 4 ),
 ( 5.700094519411444516, 6.866276094947734165 ),
 .UNSPECIFIED. ) 
 CURVE ( )  GEOMETRIC_REPRESENTATION_ITEM ( )  RATIONAL_B_SPLINE_CURVE ( ( 1.000000000000000000, 0.8898432210558864242, 0.8898432210558864242, 1.000000000000000000 ) ) 
 REPRESENTATION_ITEM ( '' )  );
#11903 = ADVANCED_FACE ( 'NONE', ( #4759 ), #16208, .T. ) ;
#11904 = CARTESIAN_POINT ( 'NONE',  ( 0.000000000000000000, 25.00000000000000355, -40.00000000000000000 ) ) ;
#11905 = CARTESIAN_POINT ( 'NONE',  ( 14.90544456622775904, 13.31698729810792692, 102.0000000000000142 ) ) ;
#11906 = CARTESIAN_POINT ( 'NONE',  ( -47.34572995173778764, 19.99999999999999645, 15.64827527265654616 ) ) ;
#11907 = CARTESIAN_POINT ( 'NONE',  ( 15.40903463028482356, 24.52187500034139589, 47.42413220539093999 ) ) ;
#11908 = CARTESIAN_POINT ( 'NONE',  ( 6.658212670116058440, 38.68388717334331517, 101.0000000000000000 ) ) ;
#11909 = CARTESIAN_POINT ( 'NONE',  ( 15.45084971874737789, 34.60000000000000853, 47.55282581475767500 ) ) ;
#11910 = CARTESIAN_POINT ( 'NONE',  ( -3.210462471511496205E-15, 29.35937500034139802, -52.43083105670540789 ) ) ;
#11911 = ADVANCED_FACE ( 'NONE', ( #3322 ), #3576, .T. ) ;
#11912 = CARTESIAN_POINT ( 'NONE',  ( 3.149380788944009968, 5.278461141749541063, 102.0000000000000142 ) ) ;
#11913 = CIRCLE ( 'NONE', #14021, 5.000000000000000000 ) ;
#11914 = ORIENTED_EDGE ( 'NONE', *, *, #2965, .F. ) ;
#11915 = EDGE_CURVE ( 'NONE', #14633, #8275, #742, .T. ) ;
#11916 = CARTESIAN_POINT ( 'NONE',  ( -3.210462471511496205E-15, 27.35937500034139447, -52.43083105670540789 ) ) ;
#11917 = VERTEX_POINT ( 'NONE', #4578 ) ;
#11918 = DIRECTION ( 'NONE',  ( 0.000000000000000000, 0.000000000000000000, -1.000000000000000000 ) ) ;
#11919 = CARTESIAN_POINT ( 'NONE',  ( 15.40903463028481113, 41.25937500034139305, -47.42413220539094709 ) ) ;
#11920 = CARTESIAN_POINT ( 'NONE',  ( 26.69586624684658105, 283.2330659412879186, 5.891732493678568439 ) ) ;
#11921 = CARTESIAN_POINT ( 'NONE',  ( -27.78424396843074362, 282.5058351977240250, 8.068487936863837362 ) ) ;
#11922 = CARTESIAN_POINT ( 'NONE',  ( 49.86468353124999453, 39.02187500034138878, -16.20201782572376459 ) ) ;
#11923 = CARTESIAN_POINT ( 'NONE',  ( -40.34137639590981905, 37.65937500034139873, -29.30972558990011478 ) ) ;
#11924 = CARTESIAN_POINT ( 'NONE',  ( -17.28626291527396930, 25.00000000000000355, -18.64048258526039703 ) ) ;
#11925 = CARTESIAN_POINT ( 'NONE',  ( -50.00000000000000000, 40.00000000000000000, 0.000000000000000000 ) ) ;
#11926 = CARTESIAN_POINT ( 'NONE',  ( 40.45084971874737079, 22.98125000068279888, -29.38926261462366440 ) ) ;
#11927 = CARTESIAN_POINT ( 'NONE',  ( -49.86468353124999453, 41.82187500034140015, -16.20201782572375393 ) ) ;
#11928 = CARTESIAN_POINT ( 'NONE',  ( -30.81806926056963292, 27.62187500034139731, -42.41743335407647209 ) ) ;
#11929 = ADVANCED_FACE ( 'NONE', ( #9736 ), #7161, .T. ) ;
#11930 = EDGE_CURVE ( 'NONE', #5627, #12134, #10204, .T. ) ;
#11931 = CARTESIAN_POINT ( 'NONE',  ( 49.86468353124999453, 46.95937500034139589, -16.20201782572376104 ) ) ;
#11932 = VERTEX_POINT ( 'NONE', #2071 ) ;
#11933 = CARTESIAN_POINT ( 'NONE',  ( -30.90169943749473802, 30.08125000068279675, 42.53254041760200721 ) ) ;
#11934 = VERTEX_POINT ( 'NONE', #16037 ) ;
#11935 = FACE_OUTER_BOUND ( 'NONE', #4737, .T. ) ;
#11936 = CARTESIAN_POINT ( 'NONE',  ( -5.000000000000000000, 61.36844557917451937, -47.78096468550220521 ) ) ;
#11937 = CARTESIAN_POINT ( 'NONE',  ( 15.40903463028481113, 43.32187500034139305, -47.42413220539094709 ) ) ;
#11938 = CARTESIAN_POINT ( 'NONE',  ( -15.40903463028480580, 26.25937500034140015, 47.42413220539094709 ) ) ;
#11939 = CARTESIAN_POINT ( 'NONE',  ( -50.00000000000000000, 39.78125000068279604, 0.000000000000000000 ) ) ;
#11940 = CARTESIAN_POINT ( 'NONE',  ( -30.81806926056962226, 42.22187500034139163, 42.41743335407647209 ) ) ;
#11941 = AXIS2_PLACEMENT_3D ( 'NONE', #5089, #6487, #12476 ) ;
#11942 = DIRECTION ( 'NONE',  ( -0.8660254037844363761, 8.780190904559507395E-17, 0.5000000000000039968 ) ) ;
#11943 = EDGE_CURVE ( 'NONE', #15320, #4733, #10307, .T. ) ;
#11944 = CARTESIAN_POINT ( 'NONE',  ( -3.210462471511496205E-15, 47.42187500034138736, -52.43083105670540789 ) ) ;
#11945 = ADVANCED_FACE ( 'NONE', ( #5994 ), #14506, .T. ) ;
#11946 = CARTESIAN_POINT ( 'NONE',  ( 0.000000000000000000, 22.50000000000000000, 101.0000000000000000 ) ) ;
#11947 = EDGE_LOOP ( 'NONE', ( #12607, #2588, #9173, #1559 ) ) ;
#11948 = CARTESIAN_POINT ( 'NONE',  ( 15.40903463028481113, 43.32187500034139305, -47.42413220539094709 ) ) ;
#11949 = ORIENTED_EDGE ( 'NONE', *, *, #12382, .F. ) ;
#11950 = EDGE_LOOP ( 'NONE', ( #4710, #6676, #10967, #349 ) ) ;
#11951 = ADVANCED_FACE ( 'NONE', ( #898 ), #16132, .F. ) ;
#11952 = DIRECTION ( 'NONE',  ( 0.000000000000000000, 0.000000000000000000, 1.000000000000000000 ) ) ;
#11953 = CARTESIAN_POINT ( 'NONE',  ( 15.45084971874737789, 38.38125000068279746, 47.55282581475767500 ) ) ;
#11954 = DIRECTION ( 'NONE',  ( 0.000000000000000000, 0.000000000000000000, 1.000000000000000000 ) ) ;
#11955 = CARTESIAN_POINT ( 'NONE',  ( 9.657523855033129090E-15, 22.50000000000000355, 52.57311121191334990 ) ) ;
#11956 = CARTESIAN_POINT ( 'NONE',  ( 15.40903463028482356, 42.45937500034140299, 47.42413220539093999 ) ) ;
#11957 = CARTESIAN_POINT ( 'NONE',  ( -40.34137639590981905, 47.65937500034139873, -29.30972558990011478 ) ) ;
#11958 = FACE_OUTER_BOUND ( 'NONE', #10653, .T. ) ;
#11959 = CARTESIAN_POINT ( 'NONE',  ( -49.99999999999999289, 45.90000000000000568, -16.24598481164531449 ) ) ;
#11960 =( NAMED_UNIT ( * ) SI_UNIT ( $, .STERADIAN. ) SOLID_ANGLE_UNIT ( ) );
#11961 = PLANE ( 'NONE',  #9136 ) ;
#11962 = CARTESIAN_POINT ( 'NONE',  ( 15.45084971874737789, 32.38125000068280457, 47.55282581475767500 ) ) ;
#11963 = DIRECTION ( 'NONE',  ( -0.6691306063588673414, 0.7431448254773861395, 0.000000000000000000 ) ) ;
#11964 = CARTESIAN_POINT ( 'NONE',  ( 15.45084971874736723, 37.40000000000000568, -47.55282581475768211 ) ) ;
#11965 = CARTESIAN_POINT ( 'NONE',  ( 40.45084971874737079, 37.20000000000000284, -29.38926261462366440 ) ) ;
#11966 = ORIENTED_EDGE ( 'NONE', *, *, #2223, .F. ) ;
#11967 = CARTESIAN_POINT ( 'NONE',  ( 49.86468353124999453, 30.95937500034139944, -16.20201782572376459 ) ) ;
#11968 = ORIENTED_EDGE ( 'NONE', *, *, #7202, .F. ) ;
#11969 = ORIENTED_EDGE ( 'NONE', *, *, #14224, .T. ) ;
#11970 = ORIENTED_EDGE ( 'NONE', *, *, #320, .F. ) ;
#11971 = CYLINDRICAL_SURFACE ( 'NONE', #9693, 50.00000000000000000 ) ;
#11972 = CARTESIAN_POINT ( 'NONE',  ( -9.189545401991425777, 24.96013318841439599, 101.0000000000000000 ) ) ;
#11973 = CARTESIAN_POINT ( 'NONE',  ( -3.210462471511496205E-15, 23.35937500034139802, -52.43083105670540789 ) ) ;
#11974 = ORIENTED_EDGE ( 'NONE', *, *, #1309, .T. ) ;
#11975 = PRODUCT_DEFINITION_SHAPE ( 'NONE', 'NONE',  #16471 ) ;
#11976 = CARTESIAN_POINT ( 'NONE',  ( -6.661118525005218949, 38.69041383028340420, 101.0000000000000000 ) ) ;
#11977 = DIRECTION ( 'NONE',  ( 0.9961946980917455452, -0.08715574274765795770, 0.000000000000000000 ) ) ;
#11978 = CARTESIAN_POINT ( 'NONE',  ( 24.14213562373094746, 282.0000000000000000, 9.571067811865477282 ) ) ;
#11979 = CARTESIAN_POINT ( 'NONE',  ( -49.86468353125000164, 29.92187500034139802, 0.000000000000000000 ) ) ;
#11980 = CARTESIAN_POINT ( 'NONE',  ( -7.919222016226816763, 29.33250428222964601, -49.99999999999999289 ) ) ;
#11981 = DIRECTION ( 'NONE',  ( 0.000000000000000000, 0.000000000000000000, -1.000000000000000000 ) ) ;
#11982 = CARTESIAN_POINT ( 'NONE',  ( -48.35726954556750457, 20.00000000000000355, 12.16803787670978387 ) ) ;
#11983 = CARTESIAN_POINT ( 'NONE',  ( 30.81806926056964002, 24.62187500034139731, 42.41743335407646498 ) ) ;
#11984 = FACE_OUTER_BOUND ( 'NONE', #6972, .T. ) ;
#11985 = CARTESIAN_POINT ( 'NONE',  ( -15.45084971874737256, 37.60000000000000142, -47.55282581475767500 ) ) ;
#11986 = CARTESIAN_POINT ( 'NONE',  ( -3.210462471511496205E-15, 25.35937500034139802, -52.43083105670540789 ) ) ;
#11987 = CARTESIAN_POINT ( 'NONE',  ( 0.000000000000000000, 193.4213562373095385, 0.000000000000000000 ) ) ;
#11988 = EDGE_LOOP ( 'NONE', ( #1564, #10463, #13374, #717 ) ) ;
#11989 = ADVANCED_FACE ( 'NONE', ( #3495 ), #8550, .F. ) ;
#11990 = CARTESIAN_POINT ( 'NONE',  ( 40.34137639590981905, 30.65937500034139518, 29.30972558990010768 ) ) ;
#11991 = VERTEX_POINT ( 'NONE', #7076 ) ;
#11992 = CARTESIAN_POINT ( 'NONE',  ( -45.58196769024076644, 258.6644603543468861, 10.00000000000000178 ) ) ;
#11994 = CARTESIAN_POINT ( 'NONE',  ( -40.34137639590981905, 43.65937500034139163, -29.30972558990011478 ) ) ;
#11993 =( BOUNDED_CURVE ( )  B_SPLINE_CURVE ( 2, ( #15364, #2399, #12790, #12545, #3905, #9055, #7647, #3821, #10139, #11464, #6235, #11306, #12875 ),
 .UNSPECIFIED., .F., .F. ) 
 B_SPLINE_CURVE_WITH_KNOTS ( ( 3, 2, 2, 2, 2, 2, 3 ),
 ( 0.4833333333333333370, 0.4866666666666666918, 0.4933333333333333459, 0.5000000000000000000, 0.5066666666666667096, 0.5133333333333333082, 0.5166666666666667185 ),
 .UNSPECIFIED. ) 
 CURVE ( )  GEOMETRIC_REPRESENTATION_ITEM ( )  RATIONAL_B_SPLINE_CURVE ( ( 0.9755282581475768211, 0.9755282581475768211, 1.000000000000000000, 0.9510565162951535312, 1.000000000000000000, 0.9510565162951535312, 1.000000000000000000, 0.9510565162951535312, 1.000000000000000000, 0.9510565162951535312, 1.000000000000000000, 0.9755282581475763770, 0.9755282581475768211 ) ) 
 REPRESENTATION_ITEM ( '' )  );
#11995 = CARTESIAN_POINT ( 'NONE',  ( 24.81239020281730490, 286.7275190727439167, 7.312390202817921292 ) ) ;
#11996 = EDGE_CURVE ( 'NONE', #15793, #5080, #15034, .T. ) ;
#11997 = ADVANCED_FACE ( 'NONE', ( #5008 ), #15851, .T. ) ;
#11998 = DIRECTION ( 'NONE',  ( -0.7071067811865484609, -0.7071067811865465735, 2.453269466693401579E-16 ) ) ;
#11999 = CARTESIAN_POINT ( 'NONE',  ( 30.81806926056964002, 30.62187500034139020, 42.41743335407647209 ) ) ;
#12000 = CARTESIAN_POINT ( 'NONE',  ( 49.86468353125001585, 34.75937500034138594, 16.20201782572375038 ) ) ;
#12001 = CARTESIAN_POINT ( 'NONE',  ( 9.395693774364776374, 21.00971865127324634, 101.0000000000000000 ) ) ;
#12002 = CARTESIAN_POINT ( 'NONE',  ( -30.81806926056963292, 27.62187500034139731, -42.41743335407647209 ) ) ;
#12003 = CARTESIAN_POINT ( 'NONE',  ( -30.90169943749473802, 40.30000000000000426, 42.53254041760200721 ) ) ;
#12004 = EDGE_CURVE ( 'NONE', #7385, #14575, #1141, .T. ) ;
#12005 = CARTESIAN_POINT ( 'NONE',  ( 40.34137639590981195, 47.05937500034140442, -29.30972558990011834 ) ) ;
#12006 = CARTESIAN_POINT ( 'NONE',  ( 9.631387414534489405E-15, 44.42187500034140157, 52.43083105670540789 ) ) ;
#12007 = CARTESIAN_POINT ( 'NONE',  ( 49.99999999999999289, 49.10000000000000853, -16.24598481164532160 ) ) ;
#12008 = EDGE_LOOP ( 'NONE', ( #4690, #11388, #5574, #3166, #11974 ) ) ;
#12009 = CARTESIAN_POINT ( 'NONE',  ( -49.86468353125000164, 45.85937500034140157, 0.000000000000000000 ) ) ;
#12010 = ORIENTED_EDGE ( 'NONE', *, *, #9677, .F. ) ;
#12011 = CARTESIAN_POINT ( 'NONE',  ( 9.657523855033129090E-15, 28.28125000068279249, 52.57311121191334990 ) ) ;
#12012 = VERTEX_POINT ( 'NONE', #15192 ) ;
#12013 = CARTESIAN_POINT ( 'NONE',  ( -30.90169943749474513, 49.48125000068279178, -42.53254041760200721 ) ) ;
#12014 = CARTESIAN_POINT ( 'NONE',  ( -49.99999999999999289, 33.88125000068280457, 16.24598481164533226 ) ) ;
#12015 = CARTESIAN_POINT ( 'NONE',  ( -15.40903463028481646, 43.52187500034139589, -47.42413220539093999 ) ) ;
#12016 = CARTESIAN_POINT ( 'NONE',  ( -40.34137639590981905, 23.65937500034139518, -29.30972558990011478 ) ) ;
#12017 = LINE ( 'NONE', #372, #2517 ) ;
#12018 = SHAPE_DEFINITION_REPRESENTATION ( #1615, #15095 ) ;
#12019 = CARTESIAN_POINT ( 'NONE',  ( 15.45084971874737789, 34.60000000000000853, 47.55282581475767500 ) ) ;
#12020 = CARTESIAN_POINT ( 'NONE',  ( 30.81806926056964002, 42.62187500034139731, 42.41743335407647209 ) ) ;
#12021 = CARTESIAN_POINT ( 'NONE',  ( 30.90169943749473802, 31.30000000000000071, -42.53254041760200721 ) ) ;
#12022 = ORIENTED_EDGE ( 'NONE', *, *, #1798, .T. ) ;
#12023 = CIRCLE ( 'NONE', #345, 17.50000000000000000 ) ;
#12024 = CARTESIAN_POINT ( 'NONE',  ( -30.81806926056962226, 40.22187500034139873, 42.41743335407647919 ) ) ;
#12025 = VERTEX_POINT ( 'NONE', #1313 ) ;
#12026 = EDGE_LOOP ( 'NONE', ( #6985, #11632, #16435, #12340 ) ) ;
#12027 = DIRECTION ( 'NONE',  ( 0.4067366430758010964, -0.9135454576426004225, 0.000000000000000000 ) ) ;
#12028 = CARTESIAN_POINT ( 'NONE',  ( 2.267949192431125027, 22.50000000000000000, 102.0000000000000142 ) ) ;
#12029 = CARTESIAN_POINT ( 'NONE',  ( -5.000000000000000000, 102.2474899284556500, -10.24748992845560380 ) ) ;
#12030 = CARTESIAN_POINT ( 'NONE',  ( 50.00000000000000711, 20.90000000000000213, 16.24598481164530739 ) ) ;
#12031 = CARTESIAN_POINT ( 'NONE',  ( -49.86468353124999453, 43.75937500034140015, -16.20201782572375393 ) ) ;
#12032 = CARTESIAN_POINT ( 'NONE',  ( 30.81806926056964002, 48.55937500034139020, 42.41743335407646498 ) ) ;
#12033 = CARTESIAN_POINT ( 'NONE',  ( 50.00000000000000000, 25.00000000000000000, -6.123233995736766085E-15 ) ) ;
#12034 = VECTOR ( 'NONE', #9802, 1000.000000000000114 ) ;
#12035 = CARTESIAN_POINT ( 'NONE',  ( 4.320770838041294581, 30.97531352606685218, 101.0000000000000000 ) ) ;
#12036 = CARTESIAN_POINT ( 'NONE',  ( 1.671572875253809487, 242.8284271247462129, -49.99999999999999289 ) ) ;
#12037 = CARTESIAN_POINT ( 'NONE',  ( -7.919222016226870942, 36.22999571913594963, 49.99999999999997158 ) ) ;
#12038 = CARTESIAN_POINT ( 'NONE',  ( -2.547328955960238000E-13, 22.28125000068279604, 49.99999999999999289 ) ) ;
#12039 = EDGE_CURVE ( 'NONE', #11084, #8347, #14033, .T. ) ;
#12040 = DIRECTION ( 'NONE',  ( 0.000000000000000000, -0.000000000000000000, -1.000000000000000000 ) ) ;
#12041 = VERTEX_POINT ( 'NONE', #2648 ) ;
#12042 = CARTESIAN_POINT ( 'NONE',  ( -49.86468353124999453, 33.95937500034139589, 16.20201782572377525 ) ) ;
#12043 = VERTEX_POINT ( 'NONE', #6324 ) ;
#12044 = ORIENTED_EDGE ( 'NONE', *, *, #12934, .T. ) ;
#12045 = ORIENTED_EDGE ( 'NONE', *, *, #12429, .F. ) ;
#12046 = TOROIDAL_SURFACE ( 'NONE', #4903, 87.81953344283027718, 2.000000000000000000 ) ;
#12047 = CIRCLE ( 'NONE', #4906, 92.05189185291139609 ) ;
#12048 = CARTESIAN_POINT ( 'NONE',  ( 50.00000000000000711, 44.68125000068278752, 16.24598481164530739 ) ) ;
#12049 = CARTESIAN_POINT ( 'NONE',  ( 9.574901606694759531E-15, 52.00000000000001421, -2.191293403013901479E-14 ) ) ;
#12050 = CARTESIAN_POINT ( 'NONE',  ( 40.34137639590981195, 23.05937500034139731, -29.30972558990011834 ) ) ;
#12051 = ORIENTED_EDGE ( 'NONE', *, *, #15914, .T. ) ;
#12052 = CARTESIAN_POINT ( 'NONE',  ( -4.126043002969710827, 5.493361027597350343, 101.0000000000000000 ) ) ;
#12053 = DIRECTION ( 'NONE',  ( 0.000000000000000000, 0.000000000000000000, 1.000000000000000000 ) ) ;
#12054 = CARTESIAN_POINT ( 'NONE',  ( -1.486087262401750042, 13.10364194761997503, 101.0000000000000000 ) ) ;
#12055 = CARTESIAN_POINT ( 'NONE',  ( -49.86468353125000164, 27.92187500034139447, 0.000000000000000000 ) ) ;
#12056 = CARTESIAN_POINT ( 'NONE',  ( -7.919222016226802552, 47.55125428154684641, -50.00000000000000000 ) ) ;
#12057 =( BOUNDED_CURVE ( )  B_SPLINE_CURVE ( 2, ( #11019, #4884, #8594, #8354, #9940, #9688, #7287, #16087, #3628, #11114, #10935, #4722, #9783 ),
 .UNSPECIFIED., .F., .T. ) 
 B_SPLINE_CURVE_WITH_KNOTS ( ( 3, 2, 2, 2, 2, 2, 3 ),
 ( 0.4500000000000000111, 0.4533333333333333104, 0.4600000000000000200, 0.4666666666666666741, 0.4733333333333333282, 0.4799999999999999822, 0.4833333333333333370 ),
 .UNSPECIFIED. ) 
 CURVE ( )  GEOMETRIC_REPRESENTATION_ITEM ( )  RATIONAL_B_SPLINE_CURVE ( ( 0.9755282581475768211, 0.9755282581475770431, 1.000000000000000000, 0.9510565162951535312, 1.000000000000000000, 0.9510565162951535312, 1.000000000000000000, 0.9510565162951535312, 1.000000000000000000, 0.9510565162951535312, 1.000000000000000000, 0.9755282581475768211, 0.9755282581475768211 ) ) 
 REPRESENTATION_ITEM ( '' )  );
#12058 = CARTESIAN_POINT ( 'NONE',  ( 2.978552182361884590E-14, 47.50000000000000711, -50.00000000000000000 ) ) ;
#12059 = DIRECTION ( 'NONE',  ( 0.000000000000000000, 1.000000000000000000, 0.000000000000000000 ) ) ;
#12060 = CARTESIAN_POINT ( 'NONE',  ( 49.86468353125001585, 24.82187500034139305, 16.20201782572375038 ) ) ;
#12061 = FACE_OUTER_BOUND ( 'NONE', #16204, .T. ) ;
#12062 = AXIS2_PLACEMENT_3D ( 'NONE', #14157, #352, #5452 ) ;
#12063 = CARTESIAN_POINT ( 'NONE',  ( -49.99999999999999289, 31.89999999999999858, -16.24598481164531449 ) ) ;
#12064 = CARTESIAN_POINT ( 'NONE',  ( 9.631387414534489405E-15, 28.35937500034139802, 52.43083105670540789 ) ) ;
#12065 = DIRECTION ( 'NONE',  ( -0.5000000000000042188, -0.000000000000000000, -0.8660254037844362651 ) ) ;
#12066 = ORIENTED_EDGE ( 'NONE', *, *, #14017, .F. ) ;
#12067 = UNCERTAINTY_MEASURE_WITH_UNIT (LENGTH_MEASURE( 1.000000000000000082E-05 ), #2386, 'distance_accuracy_value', 'NONE');
#12068 = CARTESIAN_POINT ( 'NONE',  ( 30.81806926056964002, 28.55937500034139376, 42.41743335407646498 ) ) ;
#12069 = ORIENTED_EDGE ( 'NONE', *, *, #16361, .F. ) ;
#12070 = FACE_OUTER_BOUND ( 'NONE', #9661, .T. ) ;
#12071 = CARTESIAN_POINT ( 'NONE',  ( 9.631387414534489405E-15, 44.35937500034140157, 52.43083105670540789 ) ) ;
#12072 = ADVANCED_FACE ( 'NONE', ( #11390 ), #2725, .T. ) ;
#12073 = CARTESIAN_POINT ( 'NONE',  ( 50.00000000000000000, 44.78125000068280315, -6.123233995736766085E-15 ) ) ;
#12074 = CARTESIAN_POINT ( 'NONE',  ( 49.86468353125000164, 26.92187500034139802, -6.106662507704105588E-15 ) ) ;
#12075 = CARTESIAN_POINT ( 'NONE',  ( 49.86468353124999453, 34.95937500034138878, -16.20201782572376104 ) ) ;
#12076 = DIRECTION ( 'NONE',  ( -1.000000000000000000, 0.000000000000000000, 1.734723475976807094E-17 ) ) ;
#12077 = CARTESIAN_POINT ( 'NONE',  ( -49.86468353124999453, 28.02187500034139234, 16.20201782572377525 ) ) ;
#12078 = CARTESIAN_POINT ( 'NONE',  ( -7.499999999999998224, 40.00000000000000711, -24.29058411375428150 ) ) ;
#12079 = ADVANCED_FACE ( 'NONE', ( #1231 ), #11540, .T. ) ;
#12080 = CARTESIAN_POINT ( 'NONE',  ( 9.631387414534489405E-15, 42.35937500034140157, 52.43083105670540789 ) ) ;
#12081 = CARTESIAN_POINT ( 'NONE',  ( -30.81806926056963292, 45.62187500034139020, -42.41743335407647209 ) ) ;
#12082 = AXIS2_PLACEMENT_3D ( 'NONE', #8213, #4064, #8046 ) ;
#12083 = CARTESIAN_POINT ( 'NONE',  ( 49.86468353125000164, 22.92187500034139802, -6.106662507704105588E-15 ) ) ;
#12084 = ADVANCED_FACE ( 'NONE', ( #3663 ), #2479, .T. ) ;
#12085 = PRODUCT_RELATED_PRODUCT_CATEGORY ( 'part', '', ( #15268 ) ) ;
#12087 = ORIENTED_EDGE ( 'NONE', *, *, #577, .T. ) ;
#12086 =( BOUNDED_CURVE ( )  B_SPLINE_CURVE ( 2, ( #1462, #2631, #2461, #3964, #10045, #1377, #15426, #11450, #122, #5148, #10205, #9039, #9116 ),
 .UNSPECIFIED., .F., .F. ) 
 B_SPLINE_CURVE_WITH_KNOTS ( ( 3, 2, 2, 2, 2, 2, 3 ),
 ( 0.8500000000000000888, 0.8533333333333333881, 0.8599999999999999867, 0.8666666666666666963, 0.8733333333333332948, 0.8800000000000000044, 0.8833333333333334147 ),
 .UNSPECIFIED. ) 
 CURVE ( )  GEOMETRIC_REPRESENTATION_ITEM ( )  RATIONAL_B_SPLINE_CURVE ( ( 0.9755282581475768211, 0.9755282581475771542, 1.000000000000000000, 0.9510565162951535312, 1.000000000000000000, 0.9510565162951535312, 1.000000000000000000, 0.9510565162951535312, 1.000000000000000000, 0.9510565162951535312, 1.000000000000000000, 0.9755282581475763770, 0.9755282581475768211 ) ) 
 REPRESENTATION_ITEM ( '' )  );
#12088 = CARTESIAN_POINT ( 'NONE',  ( 40.34137639590981905, 48.65937500034139873, 29.30972558990010768 ) ) ;
#12089 = EDGE_LOOP ( 'NONE', ( #7516, #15458, #16105, #14969 ) ) ;
#12090 = ORIENTED_EDGE ( 'NONE', *, *, #2216, .T. ) ;
#12091 = CARTESIAN_POINT ( 'NONE',  ( -15.45084971874737256, 33.38125000068280457, -47.55282581475767500 ) ) ;
#12092 = ORIENTED_EDGE ( 'NONE', *, *, #3820, .T. ) ;
#12093 = EDGE_CURVE ( 'NONE', #12984, #7369, #11993, .T. ) ;
#12094 = AXIS2_PLACEMENT_3D ( 'NONE', #16438, #2708, #5072 ) ;
#12095 = AXIS2_PLACEMENT_3D ( 'NONE', #14894, #12322, #10005 ) ;
#12096 = CARTESIAN_POINT ( 'NONE',  ( -40.34137639590981905, 43.72187500034139873, -29.30972558990011478 ) ) ;
#12097 = CARTESIAN_POINT ( 'NONE',  ( 15.40903463028481113, 47.32187500034140015, -47.42413220539094709 ) ) ;
#12098 =( GEOMETRIC_REPRESENTATION_CONTEXT ( 3 ) GLOBAL_UNCERTAINTY_ASSIGNED_CONTEXT ( ( #5768 ) ) GLOBAL_UNIT_ASSIGNED_CONTEXT ( ( #1799, #11773, #220 ) ) REPRESENTATION_CONTEXT ( 'NONE', 'WORKASPACE' ) );
#12099 = CARTESIAN_POINT ( 'NONE',  ( 1.293669679204937499E-13, 39.28125000068280315, -50.00000000000000000 ) ) ;
#12100 = EDGE_CURVE ( 'NONE', #691, #7234, #8886, .T. ) ;
#12101 = VECTOR ( 'NONE', #9351, 999.9999999999998863 ) ;
#12102 = CARTESIAN_POINT ( 'NONE',  ( 30.90169943749475578, 40.69999999999999574, 42.53254041760200010 ) ) ;
#12103 = CARTESIAN_POINT ( 'NONE',  ( -40.34137639590981905, 43.72187500034139873, -29.30972558990011478 ) ) ;
#12104 = CARTESIAN_POINT ( 'NONE',  ( -2.547328955960238000E-13, 30.49999999999999645, 49.99999999999999289 ) ) ;
#12105 = CIRCLE ( 'NONE', #13966, 40.00000000000000000 ) ;
#12106 = AXIS2_PLACEMENT_3D ( 'NONE', #16231, #3690, #13809 ) ;
#12107 = EDGE_LOOP ( 'NONE', ( #14125, #2566, #10135, #6237 ) ) ;
#12108 = AXIS2_PLACEMENT_3D ( 'NONE', #64, #11395, #14115 ) ;
#12109 = CARTESIAN_POINT ( 'NONE',  ( 15.40903463028481113, 45.32187500034140015, -47.42413220539094709 ) ) ;
#12110 = VERTEX_POINT ( 'NONE', #7803 ) ;
#12111 = ORIENTED_EDGE ( 'NONE', *, *, #6195, .T. ) ;
#12112 = ADVANCED_FACE ( 'NONE', ( #10060 ), #6483, .F. ) ;
#12113 = VERTEX_POINT ( 'NONE', #3985 ) ;
#12114 = DIRECTION ( 'NONE',  ( 0.000000000000000000, 0.000000000000000000, 1.000000000000000000 ) ) ;
#12115 = LINE ( 'NONE', #4560, #6803 ) ;
#12116 = CARTESIAN_POINT ( 'NONE',  ( -3.407225380398804404, 31.38205016914259105, 102.0000000000000142 ) ) ;
#12117 = CARTESIAN_POINT ( 'NONE',  ( -1.240322475938754499E-13, 36.28125000068280315, 50.00000000000000000 ) ) ;
#12118 = VECTOR ( 'NONE', #3773, 1000.000000000000114 ) ;
#12119 = AXIS2_PLACEMENT_3D ( 'NONE', #13816, #15395, #15068 ) ;
#12120 = CARTESIAN_POINT ( 'NONE',  ( 30.81806926056962936, 37.15937500034139873, -42.41743335407647209 ) ) ;
#12121 = VECTOR ( 'NONE', #9239, 1000.000000000000000 ) ;
#12122 = CARTESIAN_POINT ( 'NONE',  ( -40.34137639590981195, 46.05937500034139731, 29.30972558990012189 ) ) ;
#12123 = CARTESIAN_POINT ( 'NONE',  ( -7.919222016226816763, 29.55125428154684286, -49.99999999999999289 ) ) ;
#12124 = AXIS2_PLACEMENT_3D ( 'NONE', #6763, #12982, #14450 ) ;
#12125 = CARTESIAN_POINT ( 'NONE',  ( -49.93234176562499727, 49.96093750017070079, 0.000000000000000000 ) ) ;
#12126 = DIRECTION ( 'NONE',  ( -0.4067366430757887175, -0.9135454576426059736, 0.000000000000000000 ) ) ;
#12127 = LINE ( 'NONE', #888, #2039 ) ;
#12128 = CARTESIAN_POINT ( 'NONE',  ( -50.00000000000000000, 50.00000000000000000, 0.000000000000000000 ) ) ;
#12129 = CARTESIAN_POINT ( 'NONE',  ( 7.919222016226875382, 37.44874571845315359, -49.99999999999997158 ) ) ;
#12130 = ORIENTED_EDGE ( 'NONE', *, *, #13221, .F. ) ;
#12131 = CARTESIAN_POINT ( 'NONE',  ( -15.40903463028480580, 28.25937500034139660, 47.42413220539094709 ) ) ;
#12132 = AXIS2_PLACEMENT_3D ( 'NONE', #12726, #1077, #11242 ) ;
#12133 = VERTEX_POINT ( 'NONE', #3739 ) ;
#12134 = VERTEX_POINT ( 'NONE', #6402 ) ;
#12135 = ORIENTED_EDGE ( 'NONE', *, *, #1527, .T. ) ;
#12136 = ADVANCED_FACE ( 'NONE', ( #59 ), #5164, .T. ) ;
#12137 = AXIS2_PLACEMENT_3D ( 'NONE', #3053, #4395, #14516 ) ;
#12138 = CARTESIAN_POINT ( 'NONE',  ( 50.00000000000000000, 44.78125000068280315, -6.123233995736766085E-15 ) ) ;
#12139 = CARTESIAN_POINT ( 'NONE',  ( 7.919222016226807881, 46.55125428154685352, 50.00000000000000000 ) ) ;
#12140 = PLANE ( 'NONE',  #16326 ) ;
#12141 = ORIENTED_EDGE ( 'NONE', *, *, #9698, .F. ) ;
#12142 = CARTESIAN_POINT ( 'NONE',  ( 24.99999999999999645, 307.0000000000000568, 2.500000000000003109 ) ) ;
#12143 = FACE_OUTER_BOUND ( 'NONE', #6848, .T. ) ;
#12144 = CARTESIAN_POINT ( 'NONE',  ( 30.00000000000000355, 282.0000000000000000, -12.50000000000000000 ) ) ;
#12145 = CARTESIAN_POINT ( 'NONE',  ( 8.446640517145639571E-15, 28.49999999999999645, 50.00000000000000000 ) ) ;
#12146 = PLANE ( 'NONE',  #6211 ) ;
#12147 = CARTESIAN_POINT ( 'NONE',  ( 7.394441145214595501, 28.48516834767053751, 102.0000000000000142 ) ) ;
#12148 = CARTESIAN_POINT ( 'NONE',  ( 0.000000000000000000, 22.50000000000000000, 101.0000000000000000 ) ) ;
#12149 = CARTESIAN_POINT ( 'NONE',  ( 7.919222016226758143, 36.33250428222963535, 50.00000000000000711 ) ) ;
#12150 = CARTESIAN_POINT ( 'NONE',  ( -40.45084971874737079, 42.20000000000000284, 29.38926261462367151 ) ) ;
#12151 = CARTESIAN_POINT ( 'NONE',  ( 49.86468353124999453, 21.02187500034139589, -16.20201782572376104 ) ) ;
#12152 = PLANE ( 'NONE',  #15848 ) ;
#12153 = CARTESIAN_POINT ( 'NONE',  ( -15.45084971874737256, 29.60000000000000142, -47.55282581475767500 ) ) ;
#12154 = CARTESIAN_POINT ( 'NONE',  ( 15.40903463028482356, 28.45937500034139589, 47.42413220539093999 ) ) ;
#12155 = CARTESIAN_POINT ( 'NONE',  ( -30.90169943749473447, 30.29999999999999716, 42.53254041760200721 ) ) ;
#12156 = VERTEX_POINT ( 'NONE', #14110 ) ;
#12157 = CARTESIAN_POINT ( 'NONE',  ( 5.000000000000000000, 92.00000000000001421, 0.000000000000000000 ) ) ;
#12158 = VERTEX_POINT ( 'NONE', #10465 ) ;
#12159 = APPLICATION_CONTEXT ( 'automotive_design' ) ;
#12160 = CARTESIAN_POINT ( 'NONE',  ( 0.000000000000000000, 22.50000000000000000, 102.0000000000000142 ) ) ;
#12161 = CARTESIAN_POINT ( 'NONE',  ( -49.86468353124999453, 37.95937500034140299, 16.20201782572377525 ) ) ;
#12162 = CARTESIAN_POINT ( 'NONE',  ( -9.642970592016617104, 99.14870971539799882, 1.872989114519528986 ) ) ;
#12163 = CARTESIAN_POINT ( 'NONE',  ( 40.45084971874737789, 34.80000000000000426, 29.38926261462365375 ) ) ;
#12164 = CARTESIAN_POINT ( 'NONE',  ( 8.446640517145639571E-15, 48.49999999999999289, 50.00000000000000000 ) ) ;
#12165 = CARTESIAN_POINT ( 'NONE',  ( -49.86468353125000164, 31.92187500034139447, 0.000000000000000000 ) ) ;
#12166 = CARTESIAN_POINT ( 'NONE',  ( 40.34137639590981905, 26.65937500034139518, 29.30972558990010768 ) ) ;
#12167 = CARTESIAN_POINT ( 'NONE',  ( 8.477241335952196977, 18.18301270189230578, 102.0000000000000142 ) ) ;
#12168 = B_SPLINE_CURVE_WITH_KNOTS ( 'NONE', 3,
 ( #15161, #6532, #11597, #3787 ),
 .UNSPECIFIED., .F., .F.,
 ( 4, 4 ),
 ( 2.829004760677457000E-07, 0.001414802801989367004 ),
 .UNSPECIFIED. ) ;
#12169 = CARTESIAN_POINT ( 'NONE',  ( 49.86468353125001585, 32.82187500034139305, 16.20201782572375038 ) ) ;
#12170 = CARTESIAN_POINT ( 'NONE',  ( 15.45084971874736723, 33.39999999999999858, -47.55282581475768211 ) ) ;
#12171 = AXIS2_PLACEMENT_3D ( 'NONE', #3583, #14958, #4585 ) ;
#12172 = CARTESIAN_POINT ( 'NONE',  ( -30.81806926056962226, 48.15937500034139873, 42.41743335407647919 ) ) ;
#12173 = CARTESIAN_POINT ( 'NONE',  ( 40.34137639590981905, 38.72187500034139873, 29.30972558990010768 ) ) ;
#12174 = ADVANCED_BREP_SHAPE_REPRESENTATION ( '', ( #3320, #15812 ), #16077 ) ;
#12175 = CARTESIAN_POINT ( 'NONE',  ( -15.40903463028480580, 24.32187500034139660, 47.42413220539094709 ) ) ;
#12176 = ORIENTED_EDGE ( 'NONE', *, *, #6070, .T. ) ;
#12177 = CARTESIAN_POINT ( 'NONE',  ( -49.86468353124999453, 39.95937500034139589, 16.20201782572377169 ) ) ;
#12178 = ORIENTED_EDGE ( 'NONE', *, *, #9462, .T. ) ;
#12179 = CARTESIAN_POINT ( 'NONE',  ( 15.45084971874737789, 32.38125000068280457, 47.55282581475767500 ) ) ;
#12180 = AXIS2_PLACEMENT_3D ( 'NONE', #6584, #4930, #13793 ) ;
#12181 = ORIENTED_EDGE ( 'NONE', *, *, #14234, .T. ) ;
#12182 = CARTESIAN_POINT ( 'NONE',  ( -8.660254037844387298, 20.00000000000000355, 5.000000000000000000 ) ) ;
#12183 = CARTESIAN_POINT ( 'NONE',  ( -15.40903463028481646, 41.52187500034139589, -47.42413220539093999 ) ) ;
#12184 = CARTESIAN_POINT ( 'NONE',  ( -30.81806926056962226, 46.22187500034139163, 42.41743335407647919 ) ) ;
#12185 = LINE ( 'NONE', #13669, #13143 ) ;
#12186 = CARTESIAN_POINT ( 'NONE',  ( -3.210462471511496205E-15, 23.42187500034139802, -52.43083105670540789 ) ) ;
#12187 = CARTESIAN_POINT ( 'NONE',  ( 30.90169943749475578, 36.70000000000000995, 42.53254041760200010 ) ) ;
#12188 =( BOUNDED_CURVE ( )  B_SPLINE_CURVE ( 3, ( #12819, #1171, #88, #1340 ),
 .UNSPECIFIED., .F., .T. ) 
 B_SPLINE_CURVE_WITH_KNOTS ( ( 4, 4 ),
 ( 4.712388980384689674, 6.283185307179586232 ),
 .UNSPECIFIED. ) 
 CURVE ( )  GEOMETRIC_REPRESENTATION_ITEM ( )  RATIONAL_B_SPLINE_CURVE ( ( 1.000000000000000000, 0.8047378541243649375, 0.8047378541243649375, 1.000000000000000000 ) ) 
 REPRESENTATION_ITEM ( '' )  );
#12189 = MECHANICAL_DESIGN_GEOMETRIC_PRESENTATION_REPRESENTATION (  '', ( #7431 ), #2635 ) ;
#12190 = CARTESIAN_POINT ( 'NONE',  ( 9.631387414534489405E-15, 42.42187500034140157, 52.43083105670540789 ) ) ;
#12191 = DIRECTION ( 'NONE',  ( -0.000000000000000000, 1.000000000000000000, -0.000000000000000000 ) ) ;
#12192 = ORIENTED_EDGE ( 'NONE', *, *, #11747, .T. ) ;
#12193 = CARTESIAN_POINT ( 'NONE',  ( -40.34137639590981905, 41.72187500034139873, -29.30972558990011478 ) ) ;
#12194 = ORIENTED_EDGE ( 'NONE', *, *, #13332, .F. ) ;
#12195 = ORIENTED_EDGE ( 'NONE', *, *, #11120, .F. ) ;
#12196 = EDGE_CURVE ( 'NONE', #6735, #5387, #5481, .T. ) ;
#12197 = ORIENTED_EDGE ( 'NONE', *, *, #99, .F. ) ;
#12198 = FACE_OUTER_BOUND ( 'NONE', #13521, .T. ) ;
#12199 = LINE ( 'NONE', #16192, #2792 ) ;
#12200 = CARTESIAN_POINT ( 'NONE',  ( 2.600676159226420495E-13, 21.28125000068279604, -49.99999999999999289 ) ) ;
#12201 = CARTESIAN_POINT ( 'NONE',  ( -14.03285685708567065, 13.82077604687239258, 102.0000000000000142 ) ) ;
#12202 = AXIS2_PLACEMENT_3D ( 'NONE', #16458, #7407, #13948 ) ;
#12203 = CARTESIAN_POINT ( 'NONE',  ( 49.86468353125000164, 34.85937500034140157, -6.106662507704105588E-15 ) ) ;
#12204 = LINE ( 'NONE', #5894, #8052 ) ;
#12205 = CARTESIAN_POINT ( 'NONE',  ( -3.111920190527341144E-15, 25.50000000000000355, -50.00000000000000000 ) ) ;
#12206 = EDGE_CURVE ( 'NONE', #1863, #13641, #12962, .T. ) ;
#12207 = EDGE_CURVE ( 'NONE', #9978, #13696, #15391, .T. ) ;
#12208 = FACE_OUTER_BOUND ( 'NONE', #7965, .T. ) ;
#12209 =( LENGTH_UNIT ( ) NAMED_UNIT ( * ) SI_UNIT ( .MILLI., .METRE. ) );
#12210 = CARTESIAN_POINT ( 'NONE',  ( 17.44929222242216227, 21.16875962481693207, 101.0000000000000000 ) ) ;
#12211 = CARTESIAN_POINT ( 'NONE',  ( -40.45084971874737079, 46.20000000000000284, 29.38926261462367151 ) ) ;
#12212 = ADVANCED_FACE ( 'NONE', ( #14193 ), #11873, .T. ) ;
#12213 = DIRECTION ( 'NONE',  ( -0.000000000000000000, -1.000000000000000000, -0.000000000000000000 ) ) ;
#12214 = EDGE_LOOP ( 'NONE', ( #3073, #3199, #7686, #15920 ) ) ;
#12215 = CARTESIAN_POINT ( 'NONE',  ( -3.210462471511496205E-15, 31.35937500034139092, -52.43083105670540789 ) ) ;
#12216 = ORIENTED_EDGE ( 'NONE', *, *, #2008, .T. ) ;
#12217 = ORIENTED_EDGE ( 'NONE', *, *, #10150, .T. ) ;
#12218 = ORIENTED_EDGE ( 'NONE', *, *, #2468, .T. ) ;
#12219 = CARTESIAN_POINT ( 'NONE',  ( 50.00000000000000711, 46.68125000068278752, 16.24598481164530739 ) ) ;
#12220 = CARTESIAN_POINT ( 'NONE',  ( -50.00000000000000000, 40.00000000000000000, 0.000000000000000000 ) ) ;
#12221 = CARTESIAN_POINT ( 'NONE',  ( 7.919222016226822092, 28.55125428154684286, 49.99999999999999289 ) ) ;
#12222 = ORIENTED_EDGE ( 'NONE', *, *, #3107, .F. ) ;
#12223 = CARTESIAN_POINT ( 'NONE',  ( -20.00000000000000355, 312.0000000000000568, -2.499999999999998668 ) ) ;
#12224 = PLANE ( 'NONE',  #16443 ) ;
#12225 = CARTESIAN_POINT ( 'NONE',  ( -7.303768060548744501, 6.586594804128637293, 98.56982794341932674 ) ) ;
#12226 = FACE_OUTER_BOUND ( 'NONE', #1622, .T. ) ;
#12227 = DIRECTION ( 'NONE',  ( 0.000000000000000000, 0.000000000000000000, -1.000000000000000000 ) ) ;
#12228 = CARTESIAN_POINT ( 'NONE',  ( 45.11452830843730766, 25.00000000000000355, -21.24066852005663719 ) ) ;
#12229 = CARTESIAN_POINT ( 'NONE',  ( 0.000000000000000000, 272.0000000000000000, -82.49773270518484480 ) ) ;
#12230 = CARTESIAN_POINT ( 'NONE',  ( -7.919222016226773242, 42.44874571845315359, 50.00000000000000711 ) ) ;
#12231 = EDGE_CURVE ( 'NONE', #13242, #13993, #13041, .T. ) ;
#12232 = CARTESIAN_POINT ( 'NONE',  ( -15.40903463028481646, 25.52187500034139589, -47.42413220539093999 ) ) ;
#12233 = CARTESIAN_POINT ( 'NONE',  ( 7.500000000000000000, 40.00000000000000711, 39.29058411375427795 ) ) ;
#12234 = CARTESIAN_POINT ( 'NONE',  ( -15.45084971874736368, 26.40000000000000213, 47.55282581475768211 ) ) ;
#12235 = CARTESIAN_POINT ( 'NONE',  ( 40.34137639590981905, 26.65937500034139518, 29.30972558990010768 ) ) ;
#12236 = EDGE_CURVE ( 'NONE', #14391, #6257, #6276, .T. ) ;
#12237 = CARTESIAN_POINT ( 'NONE',  ( -15.40903463028480580, 48.25937500034140015, 47.42413220539094709 ) ) ;
#12238 = ORIENTED_EDGE ( 'NONE', *, *, #2394, .T. ) ;
#12239 = CARTESIAN_POINT ( 'NONE',  ( -15.40903463028481646, 25.45937500034139589, -47.42413220539093999 ) ) ;
#12240 = EDGE_LOOP ( 'NONE', ( #7258, #268, #6440, #9343 ) ) ;
#12241 = CARTESIAN_POINT ( 'NONE',  ( -16.79799753235266735, 27.43226914341395783, 102.0000000000000142 ) ) ;
#12242 = CARTESIAN_POINT ( 'NONE',  ( -3.210462471511496205E-15, 33.35937500034140157, -52.43083105670540789 ) ) ;
#12243 = PLANE ( 'NONE',  #3356 ) ;
#12244 = CARTESIAN_POINT ( 'NONE',  ( 25.00000000000000000, 286.6727470533782594, 2.499999999998866240 ) ) ;
#12245 = DIRECTION ( 'NONE',  ( 1.000000000000000000, 0.000000000000000000, 0.000000000000000000 ) ) ;
#12246 = CARTESIAN_POINT ( 'NONE',  ( 15.40903463028482356, 30.52187500034139589, 47.42413220539093999 ) ) ;
#12247 = CARTESIAN_POINT ( 'NONE',  ( 9.631387414534489405E-15, 28.35937500034139447, 52.43083105670540789 ) ) ;
#12248 = CARTESIAN_POINT ( 'NONE',  ( -7.919222016226870942, 36.44874571845315359, 49.99999999999997158 ) ) ;
#12249 = CARTESIAN_POINT ( 'NONE',  ( -3.210462471511496205E-15, 27.42187500034139092, -52.43083105670540789 ) ) ;
#12250 = PLANE ( 'NONE',  #14490 ) ;
#12251 = CARTESIAN_POINT ( 'NONE',  ( 49.86468353124999453, 44.95937500034139589, -16.20201782572376459 ) ) ;
#12252 = CARTESIAN_POINT ( 'NONE',  ( 15.40903463028482356, 38.52187500034139589, 47.42413220539093999 ) ) ;
#12253 = ADVANCED_FACE ( 'NONE', ( #4063 ), #13279, .T. ) ;
#12254 = CARTESIAN_POINT ( 'NONE',  ( -49.86468353124999453, 22.02187500034139589, 16.20201782572377525 ) ) ;
#12255 = EDGE_CURVE ( 'NONE', #589, #562, #387, .T. ) ;
#12256 = ORIENTED_EDGE ( 'NONE', *, *, #1740, .T. ) ;
#12257 = CARTESIAN_POINT ( 'NONE',  ( -15.40903463028481646, 39.45937500034139589, -47.42413220539093999 ) ) ;
#12258 = ORIENTED_EDGE ( 'NONE', *, *, #11744, .F. ) ;
#12259 = CARTESIAN_POINT ( 'NONE',  ( -30.90169943749473802, 24.08125000068279675, 42.53254041760200721 ) ) ;
#12260 = ORIENTED_EDGE ( 'NONE', *, *, #7525, .F. ) ;
#12261 = DIRECTION ( 'NONE',  ( 0.000000000000000000, 0.000000000000000000, 1.000000000000000000 ) ) ;
#12262 = CARTESIAN_POINT ( 'NONE',  ( -49.86468353124999453, 42.02187500034139589, 16.20201782572377169 ) ) ;
#12263 = CARTESIAN_POINT ( 'NONE',  ( -15.40903463028481646, 21.45937500034139589, -47.42413220539093999 ) ) ;
#12264 = CARTESIAN_POINT ( 'NONE',  ( 6.123233995736766085E-15, 20.00000000000000355, -50.00000000000000000 ) ) ;
#12265 = CARTESIAN_POINT ( 'NONE',  ( 40.34137639590981195, 25.12187500034139376, -29.30972558990011834 ) ) ;
#12266 = CARTESIAN_POINT ( 'NONE',  ( -30.90169943749473802, 32.08125000068280031, 42.53254041760200721 ) ) ;
#12267 = CARTESIAN_POINT ( 'NONE',  ( -3.210462471511496205E-15, 39.42187500034140157, -52.43083105670540789 ) ) ;
#12268 = CARTESIAN_POINT ( 'NONE',  ( -25.48725218878007936, 284.2907069533513322, -7.987252188781434725 ) ) ;
#12269 = ORIENTED_EDGE ( 'NONE', *, *, #8627, .T. ) ;
#12270 = CARTESIAN_POINT ( 'NONE',  ( 49.86468353124999453, 45.02187500034138878, -16.20201782572376459 ) ) ;
#12271 = CARTESIAN_POINT ( 'NONE',  ( -30.90169943749474513, 43.48125000068279178, -42.53254041760200721 ) ) ;
#12272 = ORIENTED_EDGE ( 'NONE', *, *, #9667, .F. ) ;
#12273 = ORIENTED_EDGE ( 'NONE', *, *, #14711, .T. ) ;
#12274 = PRESENTATION_LAYER_ASSIGNMENT (  '', '', ( #10950 ) ) ;
#12275 = ORIENTED_EDGE ( 'NONE', *, *, #11915, .T. ) ;
#12276 = CARTESIAN_POINT ( 'NONE',  ( -7.574663982647817484, 38.28367718720760138, 101.0000000000000000 ) ) ;
#12277 = CARTESIAN_POINT ( 'NONE',  ( -8.660254037844415720, 45.00000000000001421, -4.999999999999952927 ) ) ;
#12278 = CARTESIAN_POINT ( 'NONE',  ( -15.45084971874737256, 49.60000000000000853, -47.55282581475767500 ) ) ;
#12279 = CARTESIAN_POINT ( 'NONE',  ( 50.00000000000000000, 21.00000000000000000, -6.123233995736766085E-15 ) ) ;
#12280 = CARTESIAN_POINT ( 'NONE',  ( 30.81806926056964002, 36.55937500034139731, 42.41743335407647209 ) ) ;
#12281 = LINE ( 'NONE', #3144, #78 ) ;
#12282 = CARTESIAN_POINT ( 'NONE',  ( -30.90169943749473447, 30.29999999999999716, 42.53254041760200721 ) ) ;
#12283 = CARTESIAN_POINT ( 'NONE',  ( 37.77664397204061686, 40.00000000000000711, 13.15010152849349900 ) ) ;
#12284 = CARTESIAN_POINT ( 'NONE',  ( 1.037474003217658816E-14, 92.00000000000001421, 9.080892972013893782 ) ) ;
#12285 = DIRECTION ( 'NONE',  ( -1.000000000000000000, -1.224646799147353207E-16, 0.000000000000000000 ) ) ;
#12286 = VECTOR ( 'NONE', #2926, 1000.000000000000227 ) ;
#12287 = CARTESIAN_POINT ( 'NONE',  ( 15.45084971874737789, 36.60000000000000142, 47.55282581475767500 ) ) ;
#12288 = EDGE_LOOP ( 'NONE', ( #2090, #4231, #641 ) ) ;
#12289 = CARTESIAN_POINT ( 'NONE',  ( -49.86468353124999453, 31.95937500034139944, 16.20201782572377525 ) ) ;
#12290 = EDGE_LOOP ( 'NONE', ( #7715, #13940, #7163, #14921 ) ) ;
#12291 = ADVANCED_FACE ( 'NONE', ( #5643 ), #15768, .T. ) ;
#12292 = ORIENTED_EDGE ( 'NONE', *, *, #16095, .F. ) ;
#12293 = ORIENTED_EDGE ( 'NONE', *, *, #1527, .F. ) ;
#12294 = EDGE_CURVE ( 'NONE', #4062, #4716, #3139, .T. ) ;
#12295 = CARTESIAN_POINT ( 'NONE',  ( -50.00000000000000000, 43.78125000068280315, 0.000000000000000000 ) ) ;
#12296 = DIRECTION ( 'NONE',  ( 0.000000000000000000, 0.000000000000000000, 1.000000000000000000 ) ) ;
#12298 = ORIENTED_EDGE ( 'NONE', *, *, #2724, .F. ) ;
#12297 = CIRCLE ( 'NONE', #5154, 17.50000000000000000 ) ;
#12299 = CARTESIAN_POINT ( 'NONE',  ( -40.45084971874737789, 47.58125000068280031, -29.38926261462365730 ) ) ;
#12300 = PRESENTATION_STYLE_ASSIGNMENT (( #10976 ) ) ;
#12301 = EDGE_CURVE ( 'NONE', #6257, #14391, #11609, .T. ) ;
#12302 = LINE ( 'NONE', #2075, #2543 ) ;
#12303 = CARTESIAN_POINT ( 'NONE',  ( 1.105645237078933619E-14, 82.00000000000001421, 14.08089297201389023 ) ) ;
#12304 = DIRECTION ( 'NONE',  ( 1.000000000000000000, 0.000000000000000000, -1.734723475976807094E-17 ) ) ;
#12305 = CARTESIAN_POINT ( 'NONE',  ( 0.000000000000000000, 193.4213562373095385, 0.000000000000000000 ) ) ;
#12306 = CARTESIAN_POINT ( 'NONE',  ( 17.28626291527370284, 25.00000000000000355, -18.64048258526063151 ) ) ;
#12307 = CARTESIAN_POINT ( 'NONE',  ( -30.90169943749473447, 42.30000000000000426, 42.53254041760200721 ) ) ;
#12308 = CARTESIAN_POINT ( 'NONE',  ( -40.45084971874737079, 47.98125000068279888, 29.38926261462367151 ) ) ;
#12309 = CARTESIAN_POINT ( 'NONE',  ( 9.189545401991395579, 24.96013318841451678, 101.0000000000000000 ) ) ;
#12310 = EDGE_CURVE ( 'NONE', #326, #5251, #8425, .T. ) ;
#12311 = CARTESIAN_POINT ( 'NONE',  ( 15.45084971874737789, 28.60000000000000142, 47.55282581475767500 ) ) ;
#12312 = CARTESIAN_POINT ( 'NONE',  ( -49.86468353125000164, 25.85937500034139802, 0.000000000000000000 ) ) ;
#12313 = CARTESIAN_POINT ( 'NONE',  ( -15.45084971874736368, 44.39999999999999858, 47.55282581475768211 ) ) ;
#12314 = CIRCLE ( 'NONE', #11788, 17.50000000000000000 ) ;
#12315 = CARTESIAN_POINT ( 'NONE',  ( -16.48218589020113001, 28.38111794481753236, 101.0000000000000000 ) ) ;
#12316 = ORIENTED_EDGE ( 'NONE', *, *, #3672, .F. ) ;
#12317 = CARTESIAN_POINT ( 'NONE',  ( -2.500000000000000000, 247.0000000000000284, 44.93050188902856945 ) ) ;
#12318 = EDGE_LOOP ( 'NONE', ( #5913, #5351, #2068, #13860 ) ) ;
#12319 = DIRECTION ( 'NONE',  ( 0.9510565162951544194, -0.3090169943749448422, 0.000000000000000000 ) ) ;
#12320 = CARTESIAN_POINT ( 'NONE',  ( -15.40903463028481646, 35.45937500034139589, -47.42413220539093999 ) ) ;
#12321 = CARTESIAN_POINT ( 'NONE',  ( 1.486087262401875941, 13.10364194761998213, 102.0000000000000142 ) ) ;
#12322 = DIRECTION ( 'NONE',  ( 0.000000000000000000, 0.000000000000000000, -1.000000000000000000 ) ) ;
#12323 = CARTESIAN_POINT ( 'NONE',  ( 40.45084971874737789, 28.58125000068280031, 29.38926261462365375 ) ) ;
#12324 = AXIS2_PLACEMENT_3D ( 'NONE', #7690, #5057, #15081 ) ;
#12325 = CARTESIAN_POINT ( 'NONE',  ( 0.000000000000000000, 22.50000000000000000, 101.0000000000000000 ) ) ;
#12326 = CARTESIAN_POINT ( 'NONE',  ( -49.86468353124999453, 28.02187500034139234, 16.20201782572377525 ) ) ;
#12327 = CARTESIAN_POINT ( 'NONE',  ( -15.40903463028481646, 27.45937500034139944, -47.42413220539093999 ) ) ;
#12328 = CARTESIAN_POINT ( 'NONE',  ( 40.45084971874737079, 26.98125000068279888, -29.38926261462366440 ) ) ;
#12329 = CARTESIAN_POINT ( 'NONE',  ( -15.40903463028480580, 32.32187500034139305, 47.42413220539094709 ) ) ;
#12330 = EDGE_CURVE ( 'NONE', #9758, #3981, #8130, .T. ) ;
#12331 = CARTESIAN_POINT ( 'NONE',  ( 30.90169943749475223, 32.70000000000000284, 42.53254041760199300 ) ) ;
#12332 = CARTESIAN_POINT ( 'NONE',  ( -30.81806926056963292, 47.55937500034139731, -42.41743335407647209 ) ) ;
#12333 = CARTESIAN_POINT ( 'NONE',  ( -49.86468353125000164, 39.92187500034139447, 0.000000000000000000 ) ) ;
#12334 =( BOUNDED_CURVE ( )  B_SPLINE_CURVE ( 2, ( #2141, #5820, #2389, #9965, #11382 ),
 .UNSPECIFIED., .F., .F. ) 
 B_SPLINE_CURVE_WITH_KNOTS ( ( 3, 2, 3 ),
 ( 0.8166666666666666519, 0.8199999999999999512, 0.8260183939300572709 ),
 .UNSPECIFIED. ) 
 CURVE ( )  GEOMETRIC_REPRESENTATION_ITEM ( )  RATIONAL_B_SPLINE_CURVE ( ( 0.9755282581475768211, 0.9755282581475768211, 1.000000000000000000, 0.9558158252132341604, 0.9914069812288468508 ) ) 
 REPRESENTATION_ITEM ( '' )  );
#12335 = CARTESIAN_POINT ( 'NONE',  ( -40.34137639590981905, 21.72187500034139518, -29.30972558990011478 ) ) ;
#12336 = AXIS2_PLACEMENT_3D ( 'NONE', #3130, #6807, #2963 ) ;
#12337 = EDGE_LOOP ( 'NONE', ( #7048, #9781, #14925, #15840 ) ) ;
#12338 = AXIS2_PLACEMENT_3D ( 'NONE', #568, #1663, #14375 ) ;
#12339 = CARTESIAN_POINT ( 'NONE',  ( 49.86468353125000164, 40.85937500034139447, -6.106662507704105588E-15 ) ) ;
#12340 = ORIENTED_EDGE ( 'NONE', *, *, #15226, .T. ) ;
#12341 = CARTESIAN_POINT ( 'NONE',  ( -40.45084971874737789, 23.58125000068280031, -29.38926261462365730 ) ) ;
#12342 = ORIENTED_EDGE ( 'NONE', *, *, #12648, .F. ) ;
#12343 = CARTESIAN_POINT ( 'NONE',  ( 9.574901606694759531E-15, 52.00000000000000711, -45.00000000000002842 ) ) ;
#12344 = CARTESIAN_POINT ( 'NONE',  ( 49.86468353124999453, 33.02187500034139589, -16.20201782572376104 ) ) ;
#12345 = CARTESIAN_POINT ( 'NONE',  ( 15.40903463028482356, 20.45937500034139589, 47.42413220539093999 ) ) ;
#12346 = CARTESIAN_POINT ( 'NONE',  ( 0.000000000000000000, 102.0000000000000142, 5.000000000000000000 ) ) ;
#12347 = TOROIDAL_SURFACE ( 'NONE', #4946, 2.267949192431125027, 2.000000000000000000 ) ;
#12348 = CARTESIAN_POINT ( 'NONE',  ( -49.86468353124999453, 25.82187500034139305, -16.20201782572375393 ) ) ;
#12349 = CARTESIAN_POINT ( 'NONE',  ( -15.45084971874736368, 34.18125000068279462, 47.55282581475768211 ) ) ;
#12350 = CARTESIAN_POINT ( 'NONE',  ( 40.34137639590981905, 40.72187500034139873, 29.30972558990010768 ) ) ;
#12351 = CARTESIAN_POINT ( 'NONE',  ( -24.76951992798375102, 286.3033656649002410, -7.269519927983449037 ) ) ;
#12352 = VERTEX_POINT ( 'NONE', #1807 ) ;
#12353 = CARTESIAN_POINT ( 'NONE',  ( 40.34137639590981905, 36.72187500034139163, 29.30972558990010768 ) ) ;
#12354 = CARTESIAN_POINT ( 'NONE',  ( 19.99999999999999289, 287.0000000000000568, -7.500000000000000000 ) ) ;
#12355 = ORIENTED_EDGE ( 'NONE', *, *, #10, .T. ) ;
#12356 = EDGE_LOOP ( 'NONE', ( #15294, #4753, #366, #13842 ) ) ;
#12357 = AXIS2_PLACEMENT_3D ( 'NONE', #15886, #9495, #12053 ) ;
#12358 = ORIENTED_EDGE ( 'NONE', *, *, #8675, .F. ) ;
#12359 = STYLED_ITEM ( 'NONE', ( #6166 ), #12174 ) ;
#12360 = CARTESIAN_POINT ( 'NONE',  ( 0.000000000000000000, 25.00000000000000000, 0.000000000000000000 ) ) ;
#12361 = CARTESIAN_POINT ( 'NONE',  ( 30.27664397204019409, 40.00000000000000711, -26.14048258526078072 ) ) ;
#12362 = CARTESIAN_POINT ( 'NONE',  ( -5.000000000000000000, 99.58041009241398456, 7.580410092413952583 ) ) ;
#12363 = CARTESIAN_POINT ( 'NONE',  ( 9.227956911499398113E-15, 102.0000000000000142, -1.913737646857611713E-14 ) ) ;
#12364 = AXIS2_PLACEMENT_3D ( 'NONE', #2947, #446, #1779 ) ;
#12365 = EDGE_CURVE ( 'NONE', #15421, #243, #9720, .T. ) ;
#12366 = CARTESIAN_POINT ( 'NONE',  ( -40.34137639590981905, 39.65937500034139873, -29.30972558990011478 ) ) ;
#12367 = CARTESIAN_POINT ( 'NONE',  ( 49.86468353125001585, 42.75937500034138594, 16.20201782572375038 ) ) ;
#12368 = LINE ( 'NONE', #9803, #2905 ) ;
#12369 = PLANE ( 'NONE',  #4437 ) ;
#12370 = CLOSED_SHELL ( 'NONE', ( #6843, #13924, #14241, #6326, #15892, #5552, #15815, #5444, #4734, #9524, #1142, #2547, #4836, #6376, #12514, #12136, #13671, #1024, #1916, #723, #3997, #10836, #8422, #11176, #3793, #5323, #15167, #9896, #7638, #13011, #7720, #4895, #3371, #15249, #5423, #15789, #8760, #4471, #2886, #8329, #7123, #13666, #8859, #6559, #7204, #13048, #1632, #15243, #8794, #7230 ) ) ;
#12371 = SURFACE_STYLE_USAGE ( .BOTH. , #13287 ) ;
#12372 = VECTOR ( 'NONE', #7449, 1000.000000000000000 ) ;
#12374 = CARTESIAN_POINT ( 'NONE',  ( 0.000000000000000000, 272.0000000000000000, 0.000000000000000000 ) ) ;
#12373 = CIRCLE ( 'NONE', #7075, 45.00000000000000000 ) ;
#12375 = CIRCLE ( 'NONE', #11063, 45.00000000000000711 ) ;
#12376 = CARTESIAN_POINT ( 'NONE',  ( -50.00000000000000000, 34.00000000000000000, 0.000000000000000000 ) ) ;
#12377 = DIRECTION ( 'NONE',  ( 0.9510565162951544194, -0.3090169943749448422, 0.000000000000000000 ) ) ;
#12378 = APPLICATION_CONTEXT ( 'automotive_design' ) ;
#12379 = COLOUR_RGB ( '', 0.09019608, 0.27058824, 0.51372549) ;
#12380 = ORIENTED_EDGE ( 'NONE', *, *, #2982, .F. ) ;
#12381 = CARTESIAN_POINT ( 'NONE',  ( -49.86468353124999453, 21.95937500034138878, 16.20201782572377525 ) ) ;
#12382 = EDGE_CURVE ( 'NONE', #1101, #2974, #9463, .T. ) ;
#12383 = ORIENTED_EDGE ( 'NONE', *, *, #1806, .T. ) ;
#12384 = ORIENTED_EDGE ( 'NONE', *, *, #512, .T. ) ;
#12385 = ORIENTED_EDGE ( 'NONE', *, *, #12443, .F. ) ;
#12386 = CARTESIAN_POINT ( 'NONE',  ( 40.45084971874737789, 40.58125000068280031, 29.38926261462365375 ) ) ;
#12387 = VECTOR ( 'NONE', #342, 1000.000000000000000 ) ;
#12388 = VECTOR ( 'NONE', #5393, 1000.000000000000000 ) ;
#12389 = PRESENTATION_LAYER_ASSIGNMENT (  '', '', ( #13447 ) ) ;
#12390 = CIRCLE ( 'NONE', #14505, 45.00000000000000711 ) ;
#12391 = CARTESIAN_POINT ( 'NONE',  ( 15.45084971874737789, 46.60000000000000142, 47.55282581475767500 ) ) ;
#12392 =( LENGTH_UNIT ( ) NAMED_UNIT ( * ) SI_UNIT ( .MILLI., .METRE. ) );
#12393 = AXIS2_PLACEMENT_3D ( 'NONE', #9743, #11068, #9822 ) ;
#12394 = ORIENTED_EDGE ( 'NONE', *, *, #4622, .T. ) ;
#12395 = CARTESIAN_POINT ( 'NONE',  ( -7.919222016226804328, 48.22999571913595673, 50.00000000000000000 ) ) ;
#12396 = CARTESIAN_POINT ( 'NONE',  ( 24.78626291527397285, 40.00000000000000711, 5.650101528493621572 ) ) ;
#12397 = CARTESIAN_POINT ( 'NONE',  ( -15.72597079336059167, 14.80126021712191964, 96.11250979253432547 ) ) ;
#12398 = DIRECTION ( 'NONE',  ( 0.000000000000000000, 1.000000000000000000, 0.000000000000000000 ) ) ;
#12399 = CARTESIAN_POINT ( 'NONE',  ( 43.39327851764676325, 25.00000000000000355, -25.00490296284272773 ) ) ;
#12400 = DIRECTION ( 'NONE',  ( 0.000000000000000000, 0.000000000000000000, -1.000000000000000000 ) ) ;
#12401 = EDGE_CURVE ( 'NONE', #793, #8154, #4644, .T. ) ;
#12402 = CARTESIAN_POINT ( 'NONE',  ( -15.45084971874736368, 42.39999999999999858, 47.55282581475768211 ) ) ;
#12403 = CARTESIAN_POINT ( 'NONE',  ( -49.99999999999999289, 49.68125000068279462, -16.24598481164531449 ) ) ;
#12404 = DIRECTION ( 'NONE',  ( 0.000000000000000000, 0.000000000000000000, -1.000000000000000000 ) ) ;
#12405 = VECTOR ( 'NONE', #13213, 1000.000000000000000 ) ;
#12406 = CARTESIAN_POINT ( 'NONE',  ( 40.45084971874737789, 26.80000000000000071, 29.38926261462365375 ) ) ;
#12407 = CARTESIAN_POINT ( 'NONE',  ( 30.81806926056964002, 22.55937500034139020, 42.41743335407647209 ) ) ;
#12408 = FACE_OUTER_BOUND ( 'NONE', #3488, .T. ) ;
#12409 = AXIS2_PLACEMENT_3D ( 'NONE', #5828, #5911, #6156 ) ;
#12410 = CARTESIAN_POINT ( 'NONE',  ( -15.40903463028480580, 46.25937500034140015, 47.42413220539094709 ) ) ;
#12411 = ORIENTED_EDGE ( 'NONE', *, *, #16217, .F. ) ;
#12412 = CARTESIAN_POINT ( 'NONE',  ( 15.40903463028481113, 25.25937500034139660, -47.42413220539094709 ) ) ;
#12413 = ORIENTED_EDGE ( 'NONE', *, *, #12648, .T. ) ;
#12414 = DIRECTION ( 'NONE',  ( 0.000000000000000000, 0.000000000000000000, -1.000000000000000000 ) ) ;
#12415 = CARTESIAN_POINT ( 'NONE',  ( 30.81806926056964002, 32.55937500034139731, 42.41743335407647209 ) ) ;
#12416 = ADVANCED_FACE ( 'NONE', ( #12198 ), #16107, .F. ) ;
#12417 = CIRCLE ( 'NONE', #8959, 17.50000000000000000 ) ;
#12418 = CARTESIAN_POINT ( 'NONE',  ( 14.89925740754320493, 13.32055945583997314, 101.0000000000000000 ) ) ;
#12419 = CARTESIAN_POINT ( 'NONE',  ( 1.293669679204937499E-13, 41.28125000068279604, -50.00000000000000000 ) ) ;
#12420 = CARTESIAN_POINT ( 'NONE',  ( 7.919222016226809657, 35.44874571845314648, -50.00000000000000000 ) ) ;
#12421 = CARTESIAN_POINT ( 'NONE',  ( 30.90169943749473802, 45.08125000068280031, -42.53254041760200721 ) ) ;
#12422 = CARTESIAN_POINT ( 'NONE',  ( 40.34137639590981905, 22.72187500034139518, 29.30972558990010768 ) ) ;
#12423 = CARTESIAN_POINT ( 'NONE',  ( 30.81806926056962936, 27.15937500034139163, -42.41743335407646498 ) ) ;
#12424 = CARTESIAN_POINT ( 'NONE',  ( -3.111920190527341144E-15, 27.28125000068279604, -50.00000000000000000 ) ) ;
#12425 = CARTESIAN_POINT ( 'NONE',  ( -15.40903463028481646, 33.52187500034140299, -47.42413220539093999 ) ) ;
#12426 = CARTESIAN_POINT ( 'NONE',  ( 30.90169943749473802, 33.30000000000000426, -42.53254041760200721 ) ) ;
#12427 = CARTESIAN_POINT ( 'NONE',  ( -15.40903463028480580, 38.25937500034140015, 47.42413220539094709 ) ) ;
#12428 = CARTESIAN_POINT ( 'NONE',  ( -15.40903463028480580, 40.32187500034140015, 47.42413220539094709 ) ) ;
#12429 = EDGE_CURVE ( 'NONE', #5870, #6547, #710, .T. ) ;
#12430 = CARTESIAN_POINT ( 'NONE',  ( -49.99999999999999289, 45.89999999999999858, -16.24598481164531449 ) ) ;
#12431 = ORIENTED_EDGE ( 'NONE', *, *, #7014, .T. ) ;
#12432 = CARTESIAN_POINT ( 'NONE',  ( -3.210462471511496205E-15, 45.35937500034139447, -52.43083105670540789 ) ) ;
#12433 = VERTEX_POINT ( 'NONE', #2127 ) ;
#12434 = CARTESIAN_POINT ( 'NONE',  ( -49.99999999999999289, 21.68125000068280173, -16.24598481164531449 ) ) ;
#12435 = ORIENTED_EDGE ( 'NONE', *, *, #13167, .T. ) ;
#12436 = CARTESIAN_POINT ( 'NONE',  ( 40.45084971874737789, 40.58125000068280031, 29.38926261462365375 ) ) ;
#12437 = CARTESIAN_POINT ( 'NONE',  ( -30.81806926056963292, 39.62187500034138310, -42.41743335407647209 ) ) ;
#12438 = DIRECTION ( 'NONE',  ( 1.000000000000000000, 0.000000000000000000, 0.000000000000000000 ) ) ;
#12439 =( BOUNDED_CURVE ( )  B_SPLINE_CURVE ( 2, ( #15833, #15918, #4461, #14489, #9527, #11763, #7032, #1787, #9439, #13017, #9603, #8271, #12088, #692, #5785, #10852, #363, #4372, #4540, #14651, #1619, #8101, #6713, #3122, #6878, #5465, #531, #10531, #9282, #11931, #5626, #10688, #14336, #2953, #8020, #15744, #8193, #13260, #1860, #6955, #12009, #14990, #8681, #11014, #4620, #12432, #16169, #11192, #2361, #13579, #4878, #13499, #13413, #14906, #5952, #7367, #7445, #16079, #6037, #938, #11110, #2185, #4714, #8514, #9776, #11269, #6196, #8588, #7280, #859, #3534, #13748, #9935, #5869, #12510, #3366, #3453, #14823, #2107, #777, #1025, #16245, #2026, #4801, #1102, #7119, #9854, #13661, #6120, #2272, #12339, #3619, #16327, #7194, #4964, #9684, #10023, #3280, #8350, #12177, #10931, #15994, #14734, #8436, #12257, #2521, #267, #9093, #16416, #10181, #6616, #2609, #15154, #10342, #9015, #15076, #14150, #15232, #5050, #7761, #7685, #8842, #13825, #2768, #7843, #14072, #12920, #8763, #13903, #5372, #1526, #3705, #7601, #2686, #11351, #6444, #12832, #1436, #8929, #15406, #1351, #6365, #101, #12676, #10102, #3780, #5128, #1274, #2437, #11429, #7515, #12586, #5204, #1183, #6281, #3860, #6525, #22, #10263, #13990, #5293, #4023, #11586, #11669, #12755, #11503, #15321, #3943, #187, #3101, #14237, #5609, #4276, #4199, #6697, #11826, #9420, #9509, #4105, #5681, #10750, #8176, #15810, #4442, #14557, #1683, #11746, #13243, #6866, #1842, #3181, #9342, #11990, #9263, #9176, #10673, #13079, #14466, #8254, #6781, #13157, #13318, #1768, #14393, #435, #15653, #5537, #1919, #7012, #15726, #3014, #8004, #4356, #12068, #588, #13000, #669, #10510, #10598, #8084, #14318, #10427, #6938, #15482, #2858, #11916, #7926, #1604, #514, #348, #5447, #15573, #2938, #8416, #13482, #9662, #7422, #7101, #13727, #2089, #16057, #2341, #7177, #4689, #12239, #5933, #12412, #8569, #10996, #15976, #4524 ),
 .UNSPECIFIED., .F., .F. ) 
 B_SPLINE_CURVE_WITH_KNOTS ( ( 3, 2, 2, 2, 2, 2, 2, 2, 2, 2, 2, 2, 2, 2, 2, 2, 2, 2, 2, 2, 2, 2, 2, 2, 2, 2, 2, 2, 2, 2, 2, 2, 2, 2, 2, 2, 2, 2, 2, 2, 2, 2, 2, 2, 2, 2, 2, 2, 2, 2, 2, 2, 2, 2, 2, 2, 2, 2, 2, 2, 2, 2, 2, 2, 2, 2, 2, 2, 2, 2, 2, 2, 2, 2, 2, 2, 2, 2, 2, 2, 2, 2, 2, 2, 2, 2, 2, 2, 2, 2, 2, 2, 2, 2, 2, 2, 2, 2, 2, 2, 2, 2, 2, 2, 2, 2, 2, 2, 2, 2, 2, 2, 2, 2, 2, 2, 2, 2, 2, 2, 2, 2, 2, 2, 2, 3 ),
 ( 0.000000000000000000, 0.006666666666666667095, 0.01333333333333333419, 0.02000000000000000042, 0.02666666666666666838, 0.03333333333333333287, 0.04000000000000000083, 0.04666666666666666879, 0.05333333333333333676, 0.05999999999999999778, 0.06666666666666666574, 0.07333333333333333370, 0.08000000000000000167, 0.08666666666666666963, 0.09333333333333333759, 0.1000000000000000056, 0.1066666666666666735, 0.1133333333333333276, 0.1199999999999999956, 0.1266666666666666774, 0.1333333333333333315, 0.1400000000000000133, 0.1466666666666666674, 0.1533333333333333215, 0.1600000000000000033, 0.1666666666666666574, 0.1733333333333333393, 0.1799999999999999933, 0.1866666666666666752, 0.1933333333333333293, 0.2000000000000000111, 0.2066666666666666652, 0.2133333333333333470, 0.2200000000000000011, 0.2266666666666666552, 0.2333333333333333370, 0.2399999999999999911, 0.2466666666666666730, 0.2533333333333333548, 0.2600000000000000089, 0.2666666666666666630, 0.2733333333333333171, 0.2800000000000000266, 0.2866666666666666807, 0.2933333333333333348, 0.2999999999999999889, 0.3066666666666666430, 0.3133333333333333526, 0.3200000000000000067, 0.3266666666666666607, 0.3333333333333333148, 0.3400000000000000244, 0.3466666666666666785, 0.3533333333333333326, 0.3599999999999999867, 0.3666666666666666408, 0.3733333333333333504, 0.3800000000000000044, 0.3866666666666666585, 0.3933333333333333126, 0.4000000000000000222, 0.4066666666666666763, 0.4133333333333333304, 0.4199999999999999845, 0.4266666666666666941, 0.4333333333333333481, 0.4400000000000000022, 0.4466666666666666563, 0.4533333333333333104, 0.4600000000000000200, 0.4666666666666666741, 0.4733333333333333282, 0.4799999999999999822, 0.4866666666666666918, 0.4933333333333333459, 0.5000000000000000000, 0.5066666666666667096, 0.5133333333333333082, 0.5200000000000000178, 0.5266666666666666163, 0.5333333333333333259, 0.5400000000000000355, 0.5466666666666666341, 0.5533333333333333437, 0.5600000000000000533, 0.5666666666666666519, 0.5733333333333333615, 0.5799999999999999600, 0.5866666666666666696, 0.5933333333333333792, 0.5999999999999999778, 0.6066666666666665764, 0.6133333333333332860, 0.6200000000000001066, 0.6266666666666667052, 0.6333333333333334147, 0.6400000000000000133, 0.6466666666666667229, 0.6533333333333333215, 0.6599999999999999201, 0.6666666666666666297, 0.6733333333333332282, 0.6800000000000000488, 0.6866666666666667584, 0.6933333333333333570, 0.7000000000000000666, 0.7066666666666666652, 0.7133333333333332638, 0.7199999999999999734, 0.7266666666666665719, 0.7333333333333332815, 0.7400000000000001021, 0.7466666666666667007, 0.7533333333333334103, 0.7600000000000000089, 0.7666666666666666075, 0.7733333333333333171, 0.7799999999999999156, 0.7866666666666666252, 0.7933333333333332238, 0.8000000000000000444, 0.8066666666666667540, 0.8133333333333333526, 0.8200000000000000622, 0.8266666666666666607, 0.8286737259468953676 ),
 .UNSPECIFIED. ) 
 CURVE ( )  GEOMETRIC_REPRESENTATION_ITEM ( )  RATIONAL_B_SPLINE_CURVE ( ( 1.000000000000000000, 0.9510565162951535312, 1.000000000000000000, 0.9510565162951535312, 1.000000000000000000, 0.9510565162951535312, 1.000000000000000000, 0.9510565162951535312, 1.000000000000000000, 0.9510565162951535312, 1.000000000000000000, 0.9510565162951535312, 1.000000000000000000, 0.9510565162951535312, 1.000000000000000000, 0.9510565162951535312, 1.000000000000000000, 0.9510565162951535312, 1.000000000000000000, 0.9510565162951535312, 1.000000000000000000, 0.9510565162951535312, 1.000000000000000000, 0.9510565162951535312, 1.000000000000000000, 0.9510565162951535312, 1.000000000000000000, 0.9510565162951535312, 1.000000000000000000, 0.9510565162951535312, 1.000000000000000000, 0.9510565162951535312, 1.000000000000000000, 0.9510565162951535312, 1.000000000000000000, 0.9510565162951535312, 1.000000000000000000, 0.9510565162951535312, 1.000000000000000000, 0.9510565162951535312, 1.000000000000000000, 0.9510565162951535312, 1.000000000000000000, 0.9510565162951535312, 1.000000000000000000, 0.9510565162951535312, 1.000000000000000000, 0.9510565162951535312, 1.000000000000000000, 0.9510565162951535312, 1.000000000000000000, 0.9510565162951535312, 1.000000000000000000, 0.9510565162951535312, 1.000000000000000000, 0.9510565162951535312, 1.000000000000000000, 0.9510565162951535312, 1.000000000000000000, 0.9510565162951535312, 1.000000000000000000, 0.9510565162951535312, 1.000000000000000000, 0.9510565162951535312, 1.000000000000000000, 0.9510565162951535312, 1.000000000000000000, 0.9510565162951535312, 1.000000000000000000, 0.9510565162951535312, 1.000000000000000000, 0.9510565162951535312, 1.000000000000000000, 0.9510565162951535312, 1.000000000000000000, 0.9510565162951535312, 1.000000000000000000, 0.9510565162951535312, 1.000000000000000000, 0.9510565162951535312, 1.000000000000000000, 0.9510565162951535312, 1.000000000000000000, 0.9510565162951535312, 1.000000000000000000, 0.9510565162951535312, 1.000000000000000000, 0.9510565162951535312, 1.000000000000000000, 0.9510565162951535312, 1.000000000000000000, 0.9510565162951535312, 1.000000000000000000, 0.9510565162951535312, 1.000000000000000000, 0.9510565162951535312, 1.000000000000000000, 0.9510565162951535312, 1.000000000000000000, 0.9510565162951535312, 1.000000000000000000, 0.9510565162951535312, 1.000000000000000000, 0.9510565162951535312, 1.000000000000000000, 0.9510565162951535312, 1.000000000000000000, 0.9510565162951535312, 1.000000000000000000, 0.9510565162951535312, 1.000000000000000000, 0.9510565162951535312, 1.000000000000000000, 0.9510565162951535312, 1.000000000000000000, 0.9510565162951535312, 1.000000000000000000, 0.9510565162951535312, 1.000000000000000000, 0.9510565162951535312, 1.000000000000000000, 0.9510565162951535312, 1.000000000000000000, 0.9510565162951535312, 1.000000000000000000, 0.9510565162951535312, 1.000000000000000000, 0.9510565162951535312, 1.000000000000000000, 0.9510565162951535312, 1.000000000000000000, 0.9510565162951535312, 1.000000000000000000, 0.9510565162951535312, 1.000000000000000000, 0.9510565162951535312, 1.000000000000000000, 0.9510565162951535312, 1.000000000000000000, 0.9510565162951535312, 1.000000000000000000, 0.9510565162951535312, 1.000000000000000000, 0.9510565162951535312, 1.000000000000000000, 0.9510565162951535312, 1.000000000000000000, 0.9510565162951535312, 1.000000000000000000, 0.9510565162951535312, 1.000000000000000000, 0.9510565162951535312, 1.000000000000000000, 0.9510565162951535312, 1.000000000000000000, 0.9510565162951535312, 1.000000000000000000, 0.9510565162951535312, 1.000000000000000000, 0.9510565162951535312, 1.000000000000000000, 0.9510565162951535312, 1.000000000000000000, 0.9510565162951535312, 1.000000000000000000, 0.9510565162951535312, 1.000000000000000000, 0.9510565162951535312, 1.000000000000000000, 0.9510565162951535312, 1.000000000000000000, 0.9510565162951535312, 1.000000000000000000, 0.9510565162951535312, 1.000000000000000000, 0.9510565162951535312, 1.000000000000000000, 0.9510565162951535312, 1.000000000000000000, 0.9510565162951535312, 1.000000000000000000, 0.9510565162951535312, 1.000000000000000000, 0.9510565162951535312, 1.000000000000000000, 0.9510565162951535312, 1.000000000000000000, 0.9510565162951535312, 1.000000000000000000, 0.9510565162951535312, 1.000000000000000000, 0.9510565162951535312, 1.000000000000000000, 0.9510565162951535312, 1.000000000000000000, 0.9510565162951535312, 1.000000000000000000, 0.9510565162951535312, 1.000000000000000000, 0.9510565162951535312, 1.000000000000000000, 0.9510565162951535312, 1.000000000000000000, 0.9510565162951535312, 1.000000000000000000, 0.9510565162951535312, 1.000000000000000000, 0.9510565162951535312, 1.000000000000000000, 0.9510565162951535312, 1.000000000000000000, 0.9510565162951535312, 1.000000000000000000, 0.9510565162951535312, 1.000000000000000000, 0.9510565162951535312, 1.000000000000000000, 0.9510565162951535312, 1.000000000000000000, 0.9510565162951535312, 1.000000000000000000, 0.9510565162951535312, 1.000000000000000000, 0.9510565162951535312, 1.000000000000000000, 0.9510565162951535312, 1.000000000000000000, 0.9510565162951535312, 1.000000000000000000, 0.9510565162951535312, 1.000000000000000000, 0.9510565162951535312, 1.000000000000000000, 0.9510565162951535312, 1.000000000000000000, 0.9510565162951535312, 1.000000000000000000, 0.9510565162951535312, 1.000000000000000000, 0.9510565162951535312, 1.000000000000000000, 0.9510565162951535312, 1.000000000000000000, 0.9510565162951535312, 1.000000000000000000, 0.9510565162951535312, 1.000000000000000000, 0.9510565162951535312, 1.000000000000000000, 0.9852651290235199255, 0.9794023859079349359 ) ) 
 REPRESENTATION_ITEM ( '' )  );
#12440 = CARTESIAN_POINT ( 'NONE',  ( -40.34137639590981905, 21.72187500034139518, -29.30972558990011478 ) ) ;
#12441 = CARTESIAN_POINT ( 'NONE',  ( 15.45084971874737789, 36.38125000068279746, 47.55282581475767500 ) ) ;
#12442 = EDGE_CURVE ( 'NONE', #7423, #793, #5805, .T. ) ;
#12443 = EDGE_CURVE ( 'NONE', #12012, #15007, #5738, .T. ) ;
#12444 = CARTESIAN_POINT ( 'NONE',  ( 9.631387414534489405E-15, 36.42187500034139447, 52.43083105670540789 ) ) ;
#12445 = CARTESIAN_POINT ( 'NONE',  ( -24.98849325795416121, 282.6608420050619088, -9.994246628976297231 ) ) ;
#12446 = CARTESIAN_POINT ( 'NONE',  ( 49.86468353125000164, 36.92187500034140157, -6.106662507704105588E-15 ) ) ;
#12447 = CARTESIAN_POINT ( 'NONE',  ( 30.00000000000000355, 282.0000000000000000, -12.50000000000000000 ) ) ;
#12448 = ORIENTED_EDGE ( 'NONE', *, *, #8744, .T. ) ;
#12449 = ORIENTED_EDGE ( 'NONE', *, *, #10633, .F. ) ;
#12450 = VERTEX_POINT ( 'NONE', #8370 ) ;
#12451 = FACE_OUTER_BOUND ( 'NONE', #12872, .T. ) ;
#12452 = CARTESIAN_POINT ( 'NONE',  ( -16.48898053797772789, 28.38332565970911148, 102.0000000000000142 ) ) ;
#12453 = CARTESIAN_POINT ( 'NONE',  ( -6.668400408272873429E-15, 49.50000000000000000, -50.00000000000000000 ) ) ;
#12454 = LINE ( 'NONE', #12698, #15621 ) ;
#12455 = CARTESIAN_POINT ( 'NONE',  ( -30.81806926056963292, 37.55937500034139020, -42.41743335407647209 ) ) ;
#12456 = CARTESIAN_POINT ( 'NONE',  ( 30.81806926056962936, 41.15937500034139873, -42.41743335407646498 ) ) ;
#12457 = EDGE_CURVE ( 'NONE', #3201, #15703, #9489, .T. ) ;
#12458 = FILL_AREA_STYLE_COLOUR ( '', #10079 ) ;
#12459 = CARTESIAN_POINT ( 'NONE',  ( 15.40544456622774661, 14.18301270189236973, 102.0000000000000142 ) ) ;
#12460 = AXIS2_PLACEMENT_3D ( 'NONE', #1239, #12638, #9985 ) ;
#12461 = EDGE_CURVE ( 'NONE', #495, #2810, #16191, .T. ) ;
#12462 = CARTESIAN_POINT ( 'NONE',  ( -50.00000000000000000, 20.00000000000000000, 0.000000000000000000 ) ) ;
#12463 = CARTESIAN_POINT ( 'NONE',  ( -30.90169943749473447, 34.29999999999999005, 42.53254041760200721 ) ) ;
#12464 = CARTESIAN_POINT ( 'NONE',  ( 0.000000000000000000, 50.00000000000000000, -60.00000000000000711 ) ) ;
#12465 = ORIENTED_EDGE ( 'NONE', *, *, #716, .F. ) ;
#12466 = ADVANCED_FACE ( 'NONE', ( #720 ), #7139, .F. ) ;
#12467 = CARTESIAN_POINT ( 'NONE',  ( -40.34137639590981195, 24.05937500034139731, 29.30972558990012189 ) ) ;
#12468 = ORIENTED_EDGE ( 'NONE', *, *, #4864, .T. ) ;
#12469 = ORIENTED_EDGE ( 'NONE', *, *, #13474, .F. ) ;
#12470 = VERTEX_POINT ( 'NONE', #627 ) ;
#12471 = CARTESIAN_POINT ( 'NONE',  ( -30.90169943749473802, 40.08125000068279320, 42.53254041760200721 ) ) ;
#12472 = DIRECTION ( 'NONE',  ( 0.000000000000000000, -0.000000000000000000, 1.000000000000000000 ) ) ;
#12473 = CARTESIAN_POINT ( 'NONE',  ( 49.99999999999999289, 29.10000000000000142, -16.24598481164532160 ) ) ;
#12474 = VERTEX_POINT ( 'NONE', #9547 ) ;
#12475 = FACE_OUTER_BOUND ( 'NONE', #4310, .T. ) ;
#12476 = DIRECTION ( 'NONE',  ( 1.000000000000000000, 0.000000000000000000, 0.000000000000000000 ) ) ;
#12477 = CARTESIAN_POINT ( 'NONE',  ( -9.335200319780161848, 7.686841762321760640, 98.20306808818041588 ) ) ;
#12478 = CARTESIAN_POINT ( 'NONE',  ( 43.87482193696061472, 267.0000000000000000, 10.00000000000000178 ) ) ;
#12479 = DIRECTION ( 'NONE',  ( -0.3420201433256698231, 0.6644630243886754384, 0.6644630243886734400 ) ) ;
#12480 = CARTESIAN_POINT ( 'NONE',  ( 5.000000000000000000, 99.58041009241404140, -7.580410092414002321 ) ) ;
#12481 = DIRECTION ( 'NONE',  ( 1.000000000000000000, 0.000000000000000000, 0.000000000000000000 ) ) ;
#12482 = SURFACE_STYLE_USAGE ( .BOTH. , #68 ) ;
#12483 = CARTESIAN_POINT ( 'NONE',  ( 30.90169943749473802, 49.29999999999999716, -42.53254041760200721 ) ) ;
#12484 = CARTESIAN_POINT ( 'NONE',  ( 30.90169943749475578, 46.48125000068280599, 42.53254041760200010 ) ) ;
#12485 = PLANE ( 'NONE',  #3917 ) ;
#12486 = CARTESIAN_POINT ( 'NONE',  ( -3.219174618344376363E-15, 31.50000000000000000, -52.57311121191334990 ) ) ;
#12487 = CARTESIAN_POINT ( 'NONE',  ( -50.00000000000000000, 26.00000000000000355, 0.000000000000000000 ) ) ;
#12488 = CARTESIAN_POINT ( 'NONE',  ( 1.293669679204937499E-13, 41.28125000068279604, -50.00000000000000000 ) ) ;
#12489 = CARTESIAN_POINT ( 'NONE',  ( -49.86468353124999453, 43.75937500034140015, -16.20201782572375393 ) ) ;
#12490 = ORIENTED_EDGE ( 'NONE', *, *, #15170, .T. ) ;
#12491 = CARTESIAN_POINT ( 'NONE',  ( -5.823736356558307894E-14, 44.50000000000000000, 50.00000000000000000 ) ) ;
#12492 = EDGE_LOOP ( 'NONE', ( #13244, #3215, #8307, #13665, #7623 ) ) ;
#12493 = CARTESIAN_POINT ( 'NONE',  ( -5.988468393965924008, 15.10823117958422301, 102.0000000000000142 ) ) ;
#12494 = CARTESIAN_POINT ( 'NONE',  ( 30.81806926056962936, 37.15937500034139873, -42.41743335407647209 ) ) ;
#12495 = CARTESIAN_POINT ( 'NONE',  ( 50.00000000000000711, 40.68125000068280173, 16.24598481164530739 ) ) ;
#12496 = LINE ( 'NONE', #9533, #2804 ) ;
#12497 = CARTESIAN_POINT ( 'NONE',  ( 47.84248829804716507, 24.99999999999999289, -14.05740927763599757 ) ) ;
#12498 = CARTESIAN_POINT ( 'NONE',  ( 40.45084971874737079, 46.98125000068280599, -29.38926261462366440 ) ) ;
#12499 = CARTESIAN_POINT ( 'NONE',  ( -49.86468353124999453, 20.02187500034139589, 16.20201782572377525 ) ) ;
#12500 = CARTESIAN_POINT ( 'NONE',  ( 49.86468353125001585, 30.75937500034139305, 16.20201782572375038 ) ) ;
#12501 = DIRECTION ( 'NONE',  ( 0.000000000000000000, 0.000000000000000000, 1.000000000000000000 ) ) ;
#12502 = CARTESIAN_POINT ( 'NONE',  ( -40.34137639590981195, 36.12187500034139731, 29.30972558990012189 ) ) ;
#12503 = DIRECTION ( 'NONE',  ( 6.938893903907231459E-18, -1.000000000000000000, -5.551115123125782702E-17 ) ) ;
#12504 = CARTESIAN_POINT ( 'NONE',  ( -15.45084971874736368, 36.39999999999999858, 47.55282581475768211 ) ) ;
#12505 = CARTESIAN_POINT ( 'NONE',  ( -30.81806926056962226, 40.15937500034139163, 42.41743335407647919 ) ) ;
#12506 = CARTESIAN_POINT ( 'NONE',  ( 40.34137639590981905, 40.72187500034139873, 29.30972558990010768 ) ) ;
#12507 = ADVANCED_FACE ( 'NONE', ( #9874 ), #14926, .F. ) ;
#12508 = CARTESIAN_POINT ( 'NONE',  ( 9.657523855033129090E-15, 42.50000000000000711, 52.57311121191334990 ) ) ;
#12509 = ORIENTED_EDGE ( 'NONE', *, *, #12595, .F. ) ;
#12510 = CARTESIAN_POINT ( 'NONE',  ( 15.40903463028482356, 42.45937500034140299, 47.42413220539093999 ) ) ;
#12511 = ORIENTED_EDGE ( 'NONE', *, *, #399, .F. ) ;
#12513 = EDGE_CURVE ( 'NONE', #16149, #7285, #9710, .T. ) ;
#12512 = CARTESIAN_POINT ( 'NONE',  ( -15.45084971874736368, 24.18125000068279817, 47.55282581475768211 ) ) ;
#12514 = ADVANCED_FACE ( 'NONE', ( #4559 ), #8607, .T. ) ;
#12515 = CARTESIAN_POINT ( 'NONE',  ( 0.000000000000000000, 20.00000000000000355, 50.00000000000000000 ) ) ;
#12516 = ADVANCED_FACE ( 'NONE', ( #9622 ), #6578, .T. ) ;
#12517 = CARTESIAN_POINT ( 'NONE',  ( -3.210462471511496205E-15, 39.42187500034140157, -52.43083105670540789 ) ) ;
#12518 = CARTESIAN_POINT ( 'NONE',  ( 49.99999999999999289, 31.09999999999999787, -16.24598481164532160 ) ) ;
#12519 = CARTESIAN_POINT ( 'NONE',  ( 30.81806926056964002, 26.62187500034139731, 42.41743335407647209 ) ) ;
#12520 = CARTESIAN_POINT ( 'NONE',  ( -15.45084971874737256, 27.38125000068280102, -47.55282581475767500 ) ) ;
#12521 = ADVANCED_FACE ( 'NONE', ( #3218 ), #5972, .T. ) ;
#12522 = CARTESIAN_POINT ( 'NONE',  ( -30.81806926056962226, 32.22187500034139163, 42.41743335407647919 ) ) ;
#12523 = CARTESIAN_POINT ( 'NONE',  ( -23.90010208165381655, 283.0244618719127629, -9.450051040827696980 ) ) ;
#12524 = CARTESIAN_POINT ( 'NONE',  ( -30.81806926056962226, 34.22187500034139873, 42.41743335407647919 ) ) ;
#12525 = CARTESIAN_POINT ( 'NONE',  ( -15.45084971874737256, 41.38125000068279746, -47.55282581475767500 ) ) ;
#12526 = ORIENTED_EDGE ( 'NONE', *, *, #15226, .F. ) ;
#12527 = ORIENTED_EDGE ( 'NONE', *, *, #2657, .F. ) ;
#12528 = CARTESIAN_POINT ( 'NONE',  ( 19.99999999999999289, 287.0000000000000568, 7.500000000000002665 ) ) ;
#12529 = CARTESIAN_POINT ( 'NONE',  ( -49.86468353125000164, 49.92187500034140157, 0.000000000000000000 ) ) ;
#12530 =( BOUNDED_CURVE ( )  B_SPLINE_CURVE ( 3, ( #8951, #13922, #2539, #15340 ),
 .UNSPECIFIED., .F., .F. ) 
 B_SPLINE_CURVE_WITH_KNOTS ( ( 4, 4 ),
 ( 3.141592653589793116, 3.724683441357936609 ),
 .UNSPECIFIED. ) 
 CURVE ( )  GEOMETRIC_REPRESENTATION_ITEM ( )  RATIONAL_B_SPLINE_CURVE ( ( 1.000000000000000000, 0.9718672150731670900, 0.9718672150731670900, 1.000000000000000000 ) ) 
 REPRESENTATION_ITEM ( '' )  );
#12531 = CARTESIAN_POINT ( 'NONE',  ( -30.90169943749474513, 21.48125000068279533, -42.53254041760200721 ) ) ;
#12532 = CARTESIAN_POINT ( 'NONE',  ( 22.37674264578614114, 24.85189042352228483, 101.0000000000000000 ) ) ;
#12533 = CARTESIAN_POINT ( 'NONE',  ( -40.34137639590981905, 29.65937500034139518, -29.30972558990011478 ) ) ;
#12534 = CARTESIAN_POINT ( 'NONE',  ( 30.00000000000000000, 287.0000000000000568, 7.500000000000003553 ) ) ;
#12535 = CARTESIAN_POINT ( 'NONE',  ( 2.500000000000000000, 247.0000000000000284, -44.93050188902856945 ) ) ;
#12536 = DIRECTION ( 'NONE',  ( 1.000000000000000000, 0.000000000000000000, 0.000000000000000000 ) ) ;
#12537 = DIRECTION ( 'NONE',  ( 0.000000000000000000, 0.000000000000000000, 1.000000000000000000 ) ) ;
#12538 = SURFACE_SIDE_STYLE ('',( #3656 ) ) ;
#12539 = ORIENTED_EDGE ( 'NONE', *, *, #3871, .T. ) ;
#12540 = CARTESIAN_POINT ( 'NONE',  ( 30.81806926056964002, 24.55937500034139376, 42.41743335407647209 ) ) ;
#12541 = VERTEX_POINT ( 'NONE', #1958 ) ;
#12542 = VERTEX_POINT ( 'NONE', #1208 ) ;
#12543 = ORIENTED_EDGE ( 'NONE', *, *, #11598, .F. ) ;
#12544 = CARTESIAN_POINT ( 'NONE',  ( 40.45084971874737079, 36.98125000068279888, -29.38926261462366440 ) ) ;
#12545 = CARTESIAN_POINT ( 'NONE',  ( 30.90169943749473802, 35.08125000068278609, -42.53254041760200721 ) ) ;
#12546 = DIRECTION ( 'NONE',  ( -0.000000000000000000, 0.000000000000000000, 1.000000000000000000 ) ) ;
#12547 = ORIENTED_EDGE ( 'NONE', *, *, #9316, .T. ) ;
#12548 = CARTESIAN_POINT ( 'NONE',  ( 50.00000000000000711, 38.68125000068280173, 16.24598481164530739 ) ) ;
#12549 = CARTESIAN_POINT ( 'NONE',  ( 0.000000000000000000, 52.00000000000000711, 0.000000000000000000 ) ) ;
#12550 = CARTESIAN_POINT ( 'NONE',  ( -40.34137639590981905, 47.65937500034139873, -29.30972558990011478 ) ) ;
#12551 = CARTESIAN_POINT ( 'NONE',  ( 0.000000000000000000, 193.4213562373095385, 0.000000000000000000 ) ) ;
#12552 = CARTESIAN_POINT ( 'NONE',  ( 15.45084971874737789, 26.38125000068280102, 47.55282581475767500 ) ) ;
#12553 = CARTESIAN_POINT ( 'NONE',  ( 8.660254037844387298, 28.00000000000000355, 5.000000000000000000 ) ) ;
#12555 = LINE ( 'NONE', #16382, #6552 ) ;
#12554 = CIRCLE ( 'NONE', #53, 49.99999999999999289 ) ;
#12556 = EDGE_CURVE ( 'NONE', #3156, #14378, #3265, .T. ) ;
#12557 = DIRECTION ( 'NONE',  ( -0.000000000000000000, -1.000000000000000000, -0.000000000000000000 ) ) ;
#12558 = CARTESIAN_POINT ( 'NONE',  ( -15.45084971874737256, 47.38125000068279746, -47.55282581475767500 ) ) ;
#12559 = DIRECTION ( 'NONE',  ( -0.4067366430757887175, -0.9135454576426059736, 0.000000000000000000 ) ) ;
#12560 = CARTESIAN_POINT ( 'NONE',  ( -49.99999999999999289, 22.09999999999999787, 16.24598481164533226 ) ) ;
#12561 = CARTESIAN_POINT ( 'NONE',  ( -30.81806926056962226, 20.15937500034139518, 42.41743335407647919 ) ) ;
#12562 = CARTESIAN_POINT ( 'NONE',  ( -14.61046079763414518, 13.48729625631173867, 101.3333374614808662 ) ) ;
#12563 = CARTESIAN_POINT ( 'NONE',  ( 49.86468353125001585, 46.75937500034140015, 16.20201782572375038 ) ) ;
#12564 = ORIENTED_EDGE ( 'NONE', *, *, #10618, .T. ) ;
#12565 = AXIS2_PLACEMENT_3D ( 'NONE', #14390, #15650, #8082 ) ;
#12566 =( NAMED_UNIT ( * ) PLANE_ANGLE_UNIT ( ) SI_UNIT ( $, .RADIAN. ) );
#12567 = ORIENTED_EDGE ( 'NONE', *, *, #3150, .F. ) ;
#12568 = CARTESIAN_POINT ( 'NONE',  ( 8.446640517145639571E-15, 48.28125000068279604, 50.00000000000000000 ) ) ;
#12569 = CARTESIAN_POINT ( 'NONE',  ( -3.210462471511496205E-15, 31.35937500034139092, -52.43083105670540789 ) ) ;
#12570 = CARTESIAN_POINT ( 'NONE',  ( 7.919222016226875382, 41.22999571913594963, -49.99999999999997158 ) ) ;
#12571 = CARTESIAN_POINT ( 'NONE',  ( -45.00000000000000000, 262.0000000000000000, 0.000000000000000000 ) ) ;
#12572 = CARTESIAN_POINT ( 'NONE',  ( 47.65000835890761266, 25.00000000000000711, -14.69569212618958787 ) ) ;
#12573 = CARTESIAN_POINT ( 'NONE',  ( 15.45084971874736723, 47.18125000068280173, -47.55282581475768211 ) ) ;
#12574 = CARTESIAN_POINT ( 'NONE',  ( 30.81806926056964002, 24.62187500034139731, 42.41743335407647209 ) ) ;
#12575 = CARTESIAN_POINT ( 'NONE',  ( -15.40903463028481646, 23.45937500034139944, -47.42413220539093999 ) ) ;
#12576 = CARTESIAN_POINT ( 'NONE',  ( 30.90169943749473802, 43.30000000000000426, -42.53254041760200721 ) ) ;
#12577 = CARTESIAN_POINT ( 'NONE',  ( 30.81806926056962936, 35.22187500034138452, -42.41743335407646498 ) ) ;
#12578 = CARTESIAN_POINT ( 'NONE',  ( 2.500000000000000000, 217.0000000000000284, 44.93050188902856945 ) ) ;
#12579 = CIRCLE ( 'NONE', #1144, 45.00000000000000711 ) ;
#12580 = CARTESIAN_POINT ( 'NONE',  ( 15.45084971874736723, 37.40000000000000568, -47.55282581475768211 ) ) ;
#12581 = CARTESIAN_POINT ( 'NONE',  ( 30.81806926056962936, 39.15937500034139873, -42.41743335407647209 ) ) ;
#12582 = CARTESIAN_POINT ( 'NONE',  ( 30.81806926056962936, 31.22187500034139873, -42.41743335407647209 ) ) ;
#12583 = CARTESIAN_POINT ( 'NONE',  ( -40.45084971874737789, 47.80000000000000426, -29.38926261462365730 ) ) ;
#12584 = ORIENTED_EDGE ( 'NONE', *, *, #2739, .F. ) ;
#12585 = ADVANCED_FACE ( 'NONE', ( #12451 ), #15010, .F. ) ;
#12586 = CARTESIAN_POINT ( 'NONE',  ( 49.86468353125001585, 34.75937500034138594, 16.20201782572375038 ) ) ;
#12587 = ADVANCED_FACE ( 'NONE', ( #6303 ), #10291, .T. ) ;
#12588 = ORIENTED_EDGE ( 'NONE', *, *, #1682, .T. ) ;
#12589 = VERTEX_POINT ( 'NONE', #12528 ) ;
#12590 = CARTESIAN_POINT ( 'NONE',  ( 30.90169943749475578, 24.48125000068280244, 42.53254041760200010 ) ) ;
#12591 = CIRCLE ( 'NONE', #93, 9.080892972013911546 ) ;
#12592 = CARTESIAN_POINT ( 'NONE',  ( -0.5000000000000000000, 244.0000000000000284, -49.99999999999999289 ) ) ;
#12593 = CARTESIAN_POINT ( 'NONE',  ( 49.86468353124999453, 23.02187500034139944, -16.20201782572376459 ) ) ;
#12595 = EDGE_CURVE ( 'NONE', #8227, #13515, #7540, .T. ) ;
#12594 = FACE_OUTER_BOUND ( 'NONE', #381, .T. ) ;
#12596 = CARTESIAN_POINT ( 'NONE',  ( -49.86468353124999453, 39.82187500034140015, -16.20201782572375393 ) ) ;
#12597 = CARTESIAN_POINT ( 'NONE',  ( -43.87482193696061472, 267.0000000000000000, -10.00000000000000178 ) ) ;
#12598 = CARTESIAN_POINT ( 'NONE',  ( 9.657523855033129090E-15, 46.50000000000000711, 52.57311121191334990 ) ) ;
#12599 = CARTESIAN_POINT ( 'NONE',  ( 50.00000000000000000, 26.78125000068279959, -6.123233995736766085E-15 ) ) ;
#12600 = EDGE_CURVE ( 'NONE', #7744, #11298, #11448, .T. ) ;
#12601 = CARTESIAN_POINT ( 'NONE',  ( 14.26382420819190955, 32.65508274695842061, 93.15685069300390353 ) ) ;
#12602 = CARTESIAN_POINT ( 'NONE',  ( -49.86468353124999453, 36.02187500034139589, 16.20201782572377525 ) ) ;
#12603 = CARTESIAN_POINT ( 'NONE',  ( -25.50583519766042429, 284.7842439685843487, -3.511670395308089443 ) ) ;
#12604 = CARTESIAN_POINT ( 'NONE',  ( -30.81806926056963292, 33.62187500034139731, -42.41743335407647209 ) ) ;
#12605 = LINE ( 'NONE', #6545, #8079 ) ;
#12606 = EDGE_LOOP ( 'NONE', ( #13113, #4392, #13904, #9054, #4802, #8781, #4393, #10058, #9322, #8038, #10410, #13765, #4496, #3345, #10854, #7556, #12044, #15686, #9966, #11892 ) ) ;
#12607 = ORIENTED_EDGE ( 'NONE', *, *, #7834, .F. ) ;
#12608 = DIRECTION ( 'NONE',  ( -1.000000000000000000, 0.000000000000000000, 0.000000000000000000 ) ) ;
#12609 = DIRECTION ( 'NONE',  ( 0.8660254037844362651, 0.5000000000000041078, 0.000000000000000000 ) ) ;
#12610 = VECTOR ( 'NONE', #7322, 1000.000000000000000 ) ;
#12611 = EDGE_CURVE ( 'NONE', #9091, #2516, #7442, .T. ) ;
#12612 = CYLINDRICAL_SURFACE ( 'NONE', #7593, 45.00000000000000000 ) ;
#12613 = DIRECTION ( 'NONE',  ( 0.000000000000000000, 0.000000000000000000, 1.000000000000000000 ) ) ;
#12614 = CARTESIAN_POINT ( 'NONE',  ( -15.40903463028480580, 30.25937500034140015, 47.42413220539094709 ) ) ;
#12615 = DIRECTION ( 'NONE',  ( 0.000000000000000000, 0.000000000000000000, 1.000000000000000000 ) ) ;
#12616 = CARTESIAN_POINT ( 'NONE',  ( -49.86468353124999453, 44.02187500034139589, 16.20201782572377169 ) ) ;
#12617 = CARTESIAN_POINT ( 'NONE',  ( 14.89925740754320493, 13.32055945583997314, 101.0000000000000000 ) ) ;
#12618 = EDGE_CURVE ( 'NONE', #13297, #12621, #6311, .T. ) ;
#12619 = DIRECTION ( 'NONE',  ( -0.000000000000000000, -0.000000000000000000, -1.000000000000000000 ) ) ;
#12620 = FILL_AREA_STYLE ('',( #7228 ) ) ;
#12621 = VERTEX_POINT ( 'NONE', #1122 ) ;
#12622 = AXIS2_PLACEMENT_3D ( 'NONE', #6899, #14431, #10389 ) ;
#12623 = ADVANCED_FACE ( 'NONE', ( #8783 ), #3646, .F. ) ;
#12624 = CARTESIAN_POINT ( 'NONE',  ( 49.86468353124999453, 22.95937500034139589, -16.20201782572376459 ) ) ;
#12625 = ORIENTED_EDGE ( 'NONE', *, *, #1933, .F. ) ;
#12626 = ORIENTED_EDGE ( 'NONE', *, *, #3585, .F. ) ;
#12627 = ORIENTED_EDGE ( 'NONE', *, *, #12443, .T. ) ;
#12628 = EDGE_LOOP ( 'NONE', ( #14779, #16190, #14235, #7193 ) ) ;
#12629 =( BOUNDED_CURVE ( )  B_SPLINE_CURVE ( 2, ( #11465, #15365, #5408, #15689, #5644, #1808, #6741, #4316, #14194, #10466, #11953, #6577, #11711 ),
 .UNSPECIFIED., .F., .F. ) 
 B_SPLINE_CURVE_WITH_KNOTS ( ( 3, 2, 2, 2, 2, 2, 3 ),
 ( 0.3500000000000000333, 0.3533333333333333326, 0.3599999999999999867, 0.3666666666666666408, 0.3733333333333333504, 0.3800000000000000044, 0.3833333333333333592 ),
 .UNSPECIFIED. ) 
 CURVE ( )  GEOMETRIC_REPRESENTATION_ITEM ( )  RATIONAL_B_SPLINE_CURVE ( ( 0.9755282581475768211, 0.9755282581475770431, 1.000000000000000000, 0.9510565162951535312, 1.000000000000000000, 0.9510565162951535312, 1.000000000000000000, 0.9510565162951535312, 1.000000000000000000, 0.9510565162951535312, 1.000000000000000000, 0.9755282581475765991, 0.9755282581475768211 ) ) 
 REPRESENTATION_ITEM ( '' )  );
#12630 = DIRECTION ( 'NONE',  ( -0.9945218953682744001, 0.1045284632676435205, 0.000000000000000000 ) ) ;
#12631 = DIRECTION ( 'NONE',  ( -0.000000000000000000, 0.000000000000000000, 1.000000000000000000 ) ) ;
#12632 = CARTESIAN_POINT ( 'NONE',  ( -3.111920190527341144E-15, 29.50000000000000000, -50.00000000000000000 ) ) ;
#12633 = CARTESIAN_POINT ( 'NONE',  ( -30.90169943749474513, 37.70000000000000284, -42.53254041760200721 ) ) ;
#12634 = CARTESIAN_POINT ( 'NONE',  ( 49.86468353125001585, 48.75937500034140015, 16.20201782572375038 ) ) ;
#12635 = DIRECTION ( 'NONE',  ( 5.069245582283711292E-17, 1.000000000000000000, -8.780190904559502465E-17 ) ) ;
#12636 = AXIS2_PLACEMENT_3D ( 'NONE', #15862, #14433, #9465 ) ;
#12637 = LINE ( 'NONE', #3828, #11263 ) ;
#12638 = DIRECTION ( 'NONE',  ( 0.000000000000000000, 0.000000000000000000, 1.000000000000000000 ) ) ;
#12639 = AXIS2_PLACEMENT_3D ( 'NONE', #13469, #7243, #13791 ) ;
#12640 = AXIS2_PLACEMENT_3D ( 'NONE', #4848, #6560, #11619 ) ;
#12641 = DIRECTION ( 'NONE',  ( -0.000000000000000000, -1.000000000000000000, -0.000000000000000000 ) ) ;
#12642 = SURFACE_STYLE_USAGE ( .BOTH. , #154 ) ;
#12643 = CARTESIAN_POINT ( 'NONE',  ( 7.580410092413973011, 99.32916037694960210, 5.000000000000000000 ) ) ;
#12644 = CARTESIAN_POINT ( 'NONE',  ( 15.45084971874736723, 45.18125000068280173, -47.55282581475768211 ) ) ;
#12645 = CARTESIAN_POINT ( 'NONE',  ( 50.00000000000000000, 21.00000000000000000, -6.123233995736766085E-15 ) ) ;
#12646 = CARTESIAN_POINT ( 'NONE',  ( 9.657523855033129090E-15, 22.50000000000000355, 52.57311121191334990 ) ) ;
#12647 = DIRECTION ( 'NONE',  ( 0.000000000000000000, 1.000000000000000000, 0.000000000000000000 ) ) ;
#12648 = EDGE_CURVE ( 'NONE', #1121, #10705, #9132, .T. ) ;
#12649 = CARTESIAN_POINT ( 'NONE',  ( -14.89925740754307881, 13.32055945583976353, 101.0000000000000000 ) ) ;
#12650 = CARTESIAN_POINT ( 'NONE',  ( -15.40903463028481646, 41.45937500034140299, -47.42413220539093999 ) ) ;
#12651 = AXIS2_PLACEMENT_3D ( 'NONE', #9729, #8798, #4755 ) ;
#12652 = VERTEX_POINT ( 'NONE', #4897 ) ;
#12653 = VECTOR ( 'NONE', #5320, 1000.000000000000000 ) ;
#12654 = CIRCLE ( 'NONE', #9998, 45.00000000000000000 ) ;
#12655 = AXIS2_PLACEMENT_3D ( 'NONE', #2940, #7015, #1686 ) ;
#12656 = CARTESIAN_POINT ( 'NONE',  ( -8.660254037844387298, 20.00000000000000355, 5.000000000000000000 ) ) ;
#12657 = VERTEX_POINT ( 'NONE', #9954 ) ;
#12658 = CARTESIAN_POINT ( 'NONE',  ( 5.000000000000000000, 94.44606029984966256, 0.2275664557063671878 ) ) ;
#12659 = CARTESIAN_POINT ( 'NONE',  ( 49.86468353124999453, 26.95937500034139944, -16.20201782572376459 ) ) ;
#12660 = CARTESIAN_POINT ( 'NONE',  ( 15.45084971874737789, 26.60000000000000142, 47.55282581475767500 ) ) ;
#12661 = CARTESIAN_POINT ( 'NONE',  ( -2.869705857872620669, 39.77257016122691624, 92.94441961119122197 ) ) ;
#12662 = CARTESIAN_POINT ( 'NONE',  ( 48.24365308685505482, 25.00000000000000000, -12.61207274728973005 ) ) ;
#12663 = CARTESIAN_POINT ( 'NONE',  ( -30.81806926056962226, 36.22187500034139163, 42.41743335407647209 ) ) ;
#12664 = CARTESIAN_POINT ( 'NONE',  ( 30.90169943749475223, 30.48125000068279533, 42.53254041760199300 ) ) ;
#12665 = CARTESIAN_POINT ( 'NONE',  ( -40.34137639590981195, 20.05937500034139731, 29.30972558990012189 ) ) ;
#12666 = DIRECTION ( 'NONE',  ( 0.000000000000000000, 0.000000000000000000, 1.000000000000000000 ) ) ;
#12667 = CARTESIAN_POINT ( 'NONE',  ( -49.86468353124999453, 38.02187500034139589, 16.20201782572377169 ) ) ;
#12668 = AXIS2_PLACEMENT_3D ( 'NONE', #1412, #5031, #11560 ) ;
#12669 = DIRECTION ( 'NONE',  ( 0.000000000000000000, -1.000000000000000000, 0.000000000000000000 ) ) ;
#12670 = CARTESIAN_POINT ( 'NONE',  ( 15.45084971874737789, 30.60000000000000142, 47.55282581475767500 ) ) ;
#12671 = CARTESIAN_POINT ( 'NONE',  ( 40.34137639590981905, 36.65937500034139873, 29.30972558990010768 ) ) ;
#12672 = CARTESIAN_POINT ( 'NONE',  ( -15.40903463028480580, 30.32187500034140015, 47.42413220539094709 ) ) ;
#12673 = CARTESIAN_POINT ( 'NONE',  ( 50.00000000000000711, 46.90000000000000568, 16.24598481164530739 ) ) ;
#12674 = ORIENTED_EDGE ( 'NONE', *, *, #14806, .T. ) ;
#12675 = VERTEX_POINT ( 'NONE', #15254 ) ;
#12676 = CARTESIAN_POINT ( 'NONE',  ( -30.81806926056963292, 35.55937500034139020, -42.41743335407646498 ) ) ;
#12677 = AXIS2_PLACEMENT_3D ( 'NONE', #836, #16144, #8563 ) ;
#12678 = ORIENTED_EDGE ( 'NONE', *, *, #5523, .F. ) ;
#12679 = ORIENTED_EDGE ( 'NONE', *, *, #14672, .T. ) ;
#12680 = CARTESIAN_POINT ( 'NONE',  ( 29.50911996093742928, 282.0000000000000000, -12.00911996093662104 ) ) ;
#12682 = CARTESIAN_POINT ( 'NONE',  ( -49.86468353125000164, 45.85937500034140157, 0.000000000000000000 ) ) ;
#12681 = AXIS2_PLACEMENT_3D ( 'NONE', #472, #10388, #6659 ) ;
#12683 = CARTESIAN_POINT ( 'NONE',  ( 1.293669679204937499E-13, 39.28125000068280315, -50.00000000000000000 ) ) ;
#12684 = CARTESIAN_POINT ( 'NONE',  ( -40.34137639590981905, 21.72187500034139518, -29.30972558990011478 ) ) ;
#12685 = CARTESIAN_POINT ( 'NONE',  ( 0.000000000000000000, 272.0000000000000000, -79.49773270518484480 ) ) ;
#12686 = CARTESIAN_POINT ( 'NONE',  ( 49.86468353124999453, 43.02187500034138878, -16.20201782572376459 ) ) ;
#12687 = CARTESIAN_POINT ( 'NONE',  ( -40.45084971874737079, 25.98125000068279888, 29.38926261462367151 ) ) ;
#12688 = CARTESIAN_POINT ( 'NONE',  ( -30.81806926056962226, 20.22187500034139163, 42.41743335407647919 ) ) ;
#12689 = CARTESIAN_POINT ( 'NONE',  ( -15.45084971874737256, 29.38125000068279746, -47.55282581475767500 ) ) ;
#12690 = CARTESIAN_POINT ( 'NONE',  ( 30.81806926056962936, 49.22187500034139873, -42.41743335407647209 ) ) ;
#12691 = CARTESIAN_POINT ( 'NONE',  ( 49.86468353124999453, 35.02187500034139589, -16.20201782572376459 ) ) ;
#12692 = CARTESIAN_POINT ( 'NONE',  ( 0.000000000000000000, 272.0000000000000000, 87.81953344283027718 ) ) ;
#12693 = ORIENTED_EDGE ( 'NONE', *, *, #3159, .F. ) ;
#12694 = ORIENTED_EDGE ( 'NONE', *, *, #205, .T. ) ;
#12695 = CARTESIAN_POINT ( 'NONE',  ( -8.880528407616480990, 25.91118970470954963, 101.0000000000000000 ) ) ;
#12696 = CARTESIAN_POINT ( 'NONE',  ( 0.5000000000000001110, 38.99242250247064590, 102.0000000000000142 ) ) ;
#12697 = CARTESIAN_POINT ( 'NONE',  ( -17.50000000000000000, 22.50000000000000000, 101.0000000000000000 ) ) ;
#12698 = CARTESIAN_POINT ( 'NONE',  ( -3.149380788943775933, 5.278461141749506425, 102.0000000000000142 ) ) ;
#12699 = CARTESIAN_POINT ( 'NONE',  ( 9.631387414534489405E-15, 28.35937500034139802, 52.43083105670540789 ) ) ;
#12700 = CARTESIAN_POINT ( 'NONE',  ( 24.99999999999999645, 312.0000000000000568, 2.500000000000003109 ) ) ;
#12701 = CARTESIAN_POINT ( 'NONE',  ( -40.34137639590981905, 47.72187500034139873, -29.30972558990011478 ) ) ;
#12702 = CARTESIAN_POINT ( 'NONE',  ( -1.240322475938754499E-13, 40.50000000000000000, 50.00000000000000000 ) ) ;
#12703 = DIRECTION ( 'NONE',  ( 0.000000000000000000, 1.000000000000000000, -0.000000000000000000 ) ) ;
#12704 = CARTESIAN_POINT ( 'NONE',  ( -14.53285685708567421, 14.68680145065682474, 102.0000000000000142 ) ) ;
#12705 = ORIENTED_EDGE ( 'NONE', *, *, #9479, .F. ) ;
#12706 = EDGE_CURVE ( 'NONE', #7684, #8003, #10817, .T. ) ;
#12707 = CARTESIAN_POINT ( 'NONE',  ( 9.631387414534489405E-15, 22.35937500034139802, 52.43083105670540789 ) ) ;
#12708 = ORIENTED_EDGE ( 'NONE', *, *, #8637, .T. ) ;
#12709 = CARTESIAN_POINT ( 'NONE',  ( -15.45084971874736368, 46.18125000068280173, 47.55282581475768211 ) ) ;
#12710 = EDGE_LOOP ( 'NONE', ( #10041, #6553, #4739, #5082 ) ) ;
#12711 = ORIENTED_EDGE ( 'NONE', *, *, #6034, .T. ) ;
#12712 = CARTESIAN_POINT ( 'NONE',  ( 16.72075857324139747, 7.444561356925718520, 101.0000000000000000 ) ) ;
#12713 = CARTESIAN_POINT ( 'NONE',  ( 7.571758127758665857, 38.27715053026751946, 101.0000000000000000 ) ) ;
#12714 = ADVANCED_FACE ( 'NONE', ( #2459 ), #10043, .T. ) ;
#12715 = ADVANCED_FACE ( 'NONE', ( #13101 ), #9363, .F. ) ;
#12716 = FILL_AREA_STYLE ('',( #2815 ) ) ;
#12717 = DIRECTION ( 'NONE',  ( -0.000000000000000000, -1.000000000000000000, -0.000000000000000000 ) ) ;
#12718 = AXIS2_PLACEMENT_3D ( 'NONE', #6830, #5342, #14522 ) ;
#12719 = FACE_OUTER_BOUND ( 'NONE', #11033, .T. ) ;
#12720 = CARTESIAN_POINT ( 'NONE',  ( -7.580410092413979228, 101.3368000520362813, -5.000000000000000000 ) ) ;
#12721 = CARTESIAN_POINT ( 'NONE',  ( 1.022488062601840571E-14, 49.28125000068280315, -50.00000000000000000 ) ) ;
#12722 = CARTESIAN_POINT ( 'NONE',  ( -20.00000000000000355, 312.0000000000000568, -2.499999999999998668 ) ) ;
#12723 = EDGE_CURVE ( 'NONE', #8086, #566, #7785, .T. ) ;
#12724 = CARTESIAN_POINT ( 'NONE',  ( 0.000000000000000000, 20.00000000000000355, 0.000000000000000000 ) ) ;
#12725 = CARTESIAN_POINT ( 'NONE',  ( -49.99999999999999289, 43.68125000068279462, -16.24598481164531449 ) ) ;
#12726 = CARTESIAN_POINT ( 'NONE',  ( 0.000000000000000000, 193.4213562373095385, 0.000000000000000000 ) ) ;
#12727 = CARTESIAN_POINT ( 'NONE',  ( 30.90169943749473802, 47.08125000068280031, -42.53254041760200721 ) ) ;
#12728 = DIRECTION ( 'NONE',  ( 1.000000000000000000, 0.000000000000000000, 0.000000000000000000 ) ) ;
#12729 = VERTEX_POINT ( 'NONE', #4044 ) ;
#12730 =( BOUNDED_CURVE ( )  B_SPLINE_CURVE ( 2, ( #5083, #1640, #1390, #6736, #14106, #13038, #12959, #11631, #56, #10304, #5404, #3980, #10384 ),
 .UNSPECIFIED., .F., .F. ) 
 B_SPLINE_CURVE_WITH_KNOTS ( ( 3, 2, 2, 2, 2, 2, 3 ),
 ( 0.7833333333333333259, 0.7866666666666666252, 0.7933333333333333348, 0.8000000000000000444, 0.8066666666666666430, 0.8133333333333333526, 0.8166666666666666519 ),
 .UNSPECIFIED. ) 
 CURVE ( )  GEOMETRIC_REPRESENTATION_ITEM ( )  RATIONAL_B_SPLINE_CURVE ( ( 0.9755282581475768211, 0.9755282581475768211, 1.000000000000000000, 0.9510565162951535312, 1.000000000000000000, 0.9510565162951535312, 1.000000000000000000, 0.9510565162951535312, 1.000000000000000000, 0.9510565162951535312, 1.000000000000000000, 0.9755282581475768211, 0.9755282581475768211 ) ) 
 REPRESENTATION_ITEM ( '' )  );
#12731 = CARTESIAN_POINT ( 'NONE',  ( -30.81806926056963292, 45.55937500034139731, -42.41743335407647209 ) ) ;
#12732 = CIRCLE ( 'NONE', #6649, 88.87749532708107836 ) ;
#12733 = EDGE_LOOP ( 'NONE', ( #9918, #6322, #16033, #6441 ) ) ;
#12734 = CARTESIAN_POINT ( 'NONE',  ( 15.45084971874737789, 42.38125000068279746, 47.55282581475767500 ) ) ;
#12735 = LINE ( 'NONE', #1331, #15036 ) ;
#12736 = CARTESIAN_POINT ( 'NONE',  ( -30.81806926056962226, 26.15937500034139163, 42.41743335407647919 ) ) ;
#12737 = ORIENTED_EDGE ( 'NONE', *, *, #5847, .T. ) ;
#12738 = CARTESIAN_POINT ( 'NONE',  ( 50.00000000000000000, 33.00000000000000000, -6.123233995736766085E-15 ) ) ;
#12739 = DIRECTION ( 'NONE',  ( 0.8090169943749425663, 0.5877852522924799095, 0.000000000000000000 ) ) ;
#12740 = CARTESIAN_POINT ( 'NONE',  ( 7.394441145214595501, 28.48516834767053751, 101.0000000000000000 ) ) ;
#12741 = CARTESIAN_POINT ( 'NONE',  ( -49.86468353125000164, 33.92187500034139447, 0.000000000000000000 ) ) ;
#12742 = LINE ( 'NONE', #11490, #10533 ) ;
#12743 = VECTOR ( 'NONE', #11637, 1000.000000000000000 ) ;
#12744 = CARTESIAN_POINT ( 'NONE',  ( -3.210462471511496205E-15, 21.35937500034139447, -52.43083105670540789 ) ) ;
#12745 = CYLINDRICAL_SURFACE ( 'NONE', #480, 79.49773270518484480 ) ;
#12746 = CARTESIAN_POINT ( 'NONE',  ( -40.34137639590981905, 37.72187500034139873, -29.30972558990011478 ) ) ;
#12747 = CARTESIAN_POINT ( 'NONE',  ( -49.99999999999999289, 29.68125000068279817, -16.24598481164531449 ) ) ;
#12748 = CARTESIAN_POINT ( 'NONE',  ( -49.99999999999999289, 30.10000000000000497, 16.24598481164533226 ) ) ;
#12749 = CARTESIAN_POINT ( 'NONE',  ( 49.86468353125000164, 36.85937500034139447, -6.106662507704105588E-15 ) ) ;
#12750 = CARTESIAN_POINT ( 'NONE',  ( -49.86468353124999453, 32.02187500034139589, 16.20201782572377525 ) ) ;
#12751 = CARTESIAN_POINT ( 'NONE',  ( -40.45084971874737789, 43.80000000000000426, -29.38926261462365730 ) ) ;
#12752 = EDGE_LOOP ( 'NONE', ( #5084, #700 ) ) ;
#12753 = ORIENTED_EDGE ( 'NONE', *, *, #14017, .T. ) ;
#12754 = UNCERTAINTY_MEASURE_WITH_UNIT (LENGTH_MEASURE( 1.000000000000000082E-05 ), #15017, 'distance_accuracy_value', 'NONE');
#12755 = CARTESIAN_POINT ( 'NONE',  ( -15.40903463028481646, 33.45937500034139589, -47.42413220539093999 ) ) ;
#12756 = ORIENTED_EDGE ( 'NONE', *, *, #15358, .F. ) ;
#12757 = ORIENTED_EDGE ( 'NONE', *, *, #10794, .T. ) ;
#12758 = CARTESIAN_POINT ( 'NONE',  ( 29.01527194596313564, 282.0655843567844272, -11.51527194596550530 ) ) ;
#12759 = CARTESIAN_POINT ( 'NONE',  ( -49.86468353124999453, 45.95937500034138878, 16.20201782572377525 ) ) ;
#12760 = DIRECTION ( 'NONE',  ( 0.000000000000000000, 1.000000000000000000, 0.000000000000000000 ) ) ;
#12761 = CARTESIAN_POINT ( 'NONE',  ( 15.40903463028482356, 24.52187500034139589, 47.42413220539093999 ) ) ;
#12762 = CARTESIAN_POINT ( 'NONE',  ( -25.00000000000000355, 287.0000000000000568, 2.500000000000001332 ) ) ;
#12763 = CARTESIAN_POINT ( 'NONE',  ( 30.81806926056964002, 44.62187500034140442, 42.41743335407647209 ) ) ;
#12764 = CARTESIAN_POINT ( 'NONE',  ( -49.86468353125000164, 39.85937500034139447, 0.000000000000000000 ) ) ;
#12765 = FACE_OUTER_BOUND ( 'NONE', #14616, .T. ) ;
#12766 = CARTESIAN_POINT ( 'NONE',  ( -3.219174618344376363E-15, 47.49999999999999289, -52.57311121191334990 ) ) ;
#12767 = EDGE_CURVE ( 'NONE', #6301, #4835, #151, .T. ) ;
#12768 = CARTESIAN_POINT ( 'NONE',  ( -40.45084971874737789, 25.58125000068279675, -29.38926261462365730 ) ) ;
#12769 = FACE_OUTER_BOUND ( 'NONE', #5787, .T. ) ;
#12770 = CARTESIAN_POINT ( 'NONE',  ( 40.34137639590981905, 34.72187500034139873, 29.30972558990010768 ) ) ;
#12771 = CARTESIAN_POINT ( 'NONE',  ( -15.45084971874736368, 28.40000000000000213, 47.55282581475768211 ) ) ;
#12772 = ORIENTED_EDGE ( 'NONE', *, *, #9504, .F. ) ;
#12773 = ORIENTED_EDGE ( 'NONE', *, *, #8132, .T. ) ;
#12774 = CARTESIAN_POINT ( 'NONE',  ( 20.00000000000000000, 307.0000000000000568, -2.499999999999999556 ) ) ;
#12775 = CARTESIAN_POINT ( 'NONE',  ( 5.288637809679021457E-15, 52.00000000000001421, -35.00000000000002842 ) ) ;
#12776 = CARTESIAN_POINT ( 'NONE',  ( 0.000000000000000000, 22.50000000000000000, 102.0000000000000142 ) ) ;
#12777 = DIRECTION ( 'NONE',  ( -0.000000000000000000, 1.000000000000000000, -0.000000000000000000 ) ) ;
#12778 = CARTESIAN_POINT ( 'NONE',  ( -49.86468353124999453, 33.95937500034139589, 16.20201782572377525 ) ) ;
#12779 = CARTESIAN_POINT ( 'NONE',  ( -12.66515988160626982, 34.57657754388018390, 101.0000000000000000 ) ) ;
#12780 = CARTESIAN_POINT ( 'NONE',  ( 40.34137639590981195, 49.12187500034139731, -29.30972558990011834 ) ) ;
#12781 = CARTESIAN_POINT ( 'NONE',  ( 0.000000000000000000, 25.00000000000000355, 0.000000000000000000 ) ) ;
#12782 = CARTESIAN_POINT ( 'NONE',  ( -3.111920190527341144E-15, 35.28125000068280315, -50.00000000000000000 ) ) ;
#12783 = DIRECTION ( 'NONE',  ( -6.938893903907231459E-18, 1.000000000000000000, 5.551115123125782702E-17 ) ) ;
#12784 = VERTEX_POINT ( 'NONE', #456 ) ;
#12785 = CARTESIAN_POINT ( 'NONE',  ( -40.34137639590981195, 48.12187500034139731, 29.30972558990012189 ) ) ;
#12786 = EDGE_LOOP ( 'NONE', ( #10490, #3070, #15439, #15917 ) ) ;
#12787 = CARTESIAN_POINT ( 'NONE',  ( 7.580410092413973011, 101.3368000520362813, 5.000000000000000000 ) ) ;
#12788 = ORIENTED_EDGE ( 'NONE', *, *, #2598, .T. ) ;
#12789 = ORIENTED_EDGE ( 'NONE', *, *, #10540, .T. ) ;
#12790 = CARTESIAN_POINT ( 'NONE',  ( 15.45084971874736723, 35.18125000068280173, -47.55282581475768211 ) ) ;
#12791 = DIRECTION ( 'NONE',  ( -2.312964634635742464E-16, -0.000000000000000000, 1.000000000000000000 ) ) ;
#12792 = SURFACE_STYLE_FILL_AREA ( #12716 ) ;
#12793 = CARTESIAN_POINT ( 'NONE',  ( 0.000000000000000000, 25.00000000000000000, 0.000000000000000000 ) ) ;
#12794 = CARTESIAN_POINT ( 'NONE',  ( -49.86468353124999453, 49.75937500034138594, -16.20201782572375393 ) ) ;
#12795 = FACE_OUTER_BOUND ( 'NONE', #7963, .T. ) ;
#12796 = CARTESIAN_POINT ( 'NONE',  ( 1.790468199911986025, 98.25246584726779986, -9.080892972013931086 ) ) ;
#12797 = CARTESIAN_POINT ( 'NONE',  ( 36.11321354817260953, 29.97008732934370201, -17.92868204048114222 ) ) ;
#12798 =( LENGTH_UNIT ( ) NAMED_UNIT ( * ) SI_UNIT ( .MILLI., .METRE. ) );
#12799 = CARTESIAN_POINT ( 'NONE',  ( 10.49054022437463018, 8.911660907547437560, 101.3333374614808662 ) ) ;
#12800 = CARTESIAN_POINT ( 'NONE',  ( 50.00000000000000711, 38.68125000068280173, 16.24598481164530739 ) ) ;
#12801 = CARTESIAN_POINT ( 'NONE',  ( 30.90169943749475223, 44.48125000068279888, 42.53254041760199300 ) ) ;
#12802 = CARTESIAN_POINT ( 'NONE',  ( -15.45084971874736368, 24.40000000000000213, 47.55282581475768211 ) ) ;
#12803 = LINE ( 'NONE', #6673, #8822 ) ;
#12804 = ADVANCED_FACE ( 'NONE', ( #12855 ), #7344, .T. ) ;
#12805 = VERTEX_POINT ( 'NONE', #9114 ) ;
#12806 = CARTESIAN_POINT ( 'NONE',  ( 49.86468353125000164, 38.85937500034139447, -6.106662507704105588E-15 ) ) ;
#12807 = ORIENTED_EDGE ( 'NONE', *, *, #9049, .F. ) ;
#12808 = CARTESIAN_POINT ( 'NONE',  ( 5.000000000000000000, 90.58578643762692195, 1.414213562373097588 ) ) ;
#12809 = EDGE_CURVE ( 'NONE', #5951, #12657, #1459, .T. ) ;
#12810 = CARTESIAN_POINT ( 'NONE',  ( 5.988468393966018155, 15.10823117958429584, 101.0000000000000000 ) ) ;
#12811 = CARTESIAN_POINT ( 'NONE',  ( -49.86468353124999453, 27.95937500034139944, 16.20201782572377525 ) ) ;
#12813 = EDGE_LOOP ( 'NONE', ( #6462, #7687, #6921, #4463 ) ) ;
#12812 = CIRCLE ( 'NONE', #586, 45.00000000000000711 ) ;
#12814 = CARTESIAN_POINT ( 'NONE',  ( 7.919222016226693306, 32.55125428154685352, 50.00000000000003553 ) ) ;
#12815 = DIRECTION ( 'NONE',  ( -0.5877852522924797984, 0.8090169943749424553, 0.000000000000000000 ) ) ;
#12816 = CARTESIAN_POINT ( 'NONE',  ( 47.02241032844496971, 25.00000000000000000, -16.59456509147096881 ) ) ;
#12817 = CARTESIAN_POINT ( 'NONE',  ( -30.81806926056963292, 31.62187500034140086, -42.41743335407646498 ) ) ;
#12818 = EDGE_CURVE ( 'NONE', #13297, #11113, #3077, .T. ) ;
#12819 = CARTESIAN_POINT ( 'NONE',  ( 30.00000000000000355, 282.0000000000000000, -12.50000000000000000 ) ) ;
#12820 = CARTESIAN_POINT ( 'NONE',  ( 9.631387414534489405E-15, 22.35937500034139802, 52.43083105670540789 ) ) ;
#12821 = LINE ( 'NONE', #13980, #14765 ) ;
#12822 = CARTESIAN_POINT ( 'NONE',  ( -40.34137639590981195, 30.12187500034139731, 29.30972558990012189 ) ) ;
#12823 =( BOUNDED_CURVE ( )  B_SPLINE_CURVE ( 2, ( #12205, #13688, #3224, #807, #3562, #9881, #13364 ),
 .UNSPECIFIED., .F., .F. ) 
 B_SPLINE_CURVE_WITH_KNOTS ( ( 3, 2, 2, 3 ),
 ( 0.8166666666666666519, 0.8199999999999999512, 0.8266666666666666607, 0.8333333333333333703 ),
 .UNSPECIFIED. ) 
 CURVE ( )  GEOMETRIC_REPRESENTATION_ITEM ( )  RATIONAL_B_SPLINE_CURVE ( ( 0.9755282581475768211, 0.9755282581475768211, 1.000000000000000000, 0.9510565162951535312, 1.000000000000000000, 0.9510565162951535312, 1.000000000000000000 ) ) 
 REPRESENTATION_ITEM ( '' )  );
#12824 = FACE_OUTER_BOUND ( 'NONE', #9892, .T. ) ;
#12825 = CARTESIAN_POINT ( 'NONE',  ( 15.45084971874736723, 29.40000000000000213, -47.55282581475768211 ) ) ;
#12826 = CARTESIAN_POINT ( 'NONE',  ( 49.86468353124999453, 32.95937500034138168, -16.20201782572376459 ) ) ;
#12827 = CARTESIAN_POINT ( 'NONE',  ( -15.40903463028481646, 31.52187500034139944, -47.42413220539093999 ) ) ;
#12828 = VECTOR ( 'NONE', #12065, 1000.000000000000114 ) ;
#12829 = CARTESIAN_POINT ( 'NONE',  ( -30.90169943749474868, 41.70000000000000284, -42.53254041760200721 ) ) ;
#12830 = ORIENTED_EDGE ( 'NONE', *, *, #15742, .F. ) ;
#12831 = EDGE_CURVE ( 'NONE', #14610, #9620, #6717, .T. ) ;
#12832 = CARTESIAN_POINT ( 'NONE',  ( -15.40903463028480580, 36.25937500034140015, 47.42413220539094709 ) ) ;
#12833 = ORIENTED_EDGE ( 'NONE', *, *, #8150, .F. ) ;
#12834 = ORIENTED_EDGE ( 'NONE', *, *, #10208, .T. ) ;
#12835 = CARTESIAN_POINT ( 'NONE',  ( 24.86904120090366277, 286.8604097559505703, -7.369041200904232092 ) ) ;
#12836 = CARTESIAN_POINT ( 'NONE',  ( 9.631387414534489405E-15, 46.35937500034139447, 52.43083105670540789 ) ) ;
#12837 = PLANE ( 'NONE',  #12324 ) ;
#12838 = CARTESIAN_POINT ( 'NONE',  ( -49.86468353124999453, 25.82187500034139305, -16.20201782572375393 ) ) ;
#12839 = EDGE_CURVE ( 'NONE', #8062, #332, #11902, .T. ) ;
#12840 = AXIS2_PLACEMENT_3D ( 'NONE', #1905, #14874, #5755 ) ;
#12841 = FACE_OUTER_BOUND ( 'NONE', #10537, .T. ) ;
#12842 = CARTESIAN_POINT ( 'NONE',  ( 49.86468353125001585, 34.82187500034140015, 16.20201782572375038 ) ) ;
#12843 = CARTESIAN_POINT ( 'NONE',  ( -40.34137639590981905, 41.65937500034139873, -29.30972558990011478 ) ) ;
#12844 = CARTESIAN_POINT ( 'NONE',  ( -7.919222016226838967, 44.44874571845315359, 49.99999999999999289 ) ) ;
#12845 = CARTESIAN_POINT ( 'NONE',  ( -49.99999999999999289, 47.89999999999999858, -16.24598481164531449 ) ) ;
#12846 = CARTESIAN_POINT ( 'NONE',  ( 49.99999999999999289, 28.88125000068279391, -16.24598481164532160 ) ) ;
#12847 = CARTESIAN_POINT ( 'NONE',  ( 11.57959921299713457, 35.63367363361179230, 92.99972171590198400 ) ) ;
#12848 = CARTESIAN_POINT ( 'NONE',  ( 49.86468353124999453, 29.02187500034139234, -16.20201782572376459 ) ) ;
#12849 = EDGE_CURVE ( 'NONE', #15936, #11630, #10839, .T. ) ;
#12850 = AXIS2_PLACEMENT_3D ( 'NONE', #12781, #6072, #8618 ) ;
#12851 = DIRECTION ( 'NONE',  ( 1.000000000000000000, -0.000000000000000000, -0.000000000000000000 ) ) ;
#12852 = EDGE_LOOP ( 'NONE', ( #4642, #11427, #10895, #4917 ) ) ;
#12853 = CARTESIAN_POINT ( 'NONE',  ( 50.00000000000000711, 36.68125000068280173, 16.24598481164530739 ) ) ;
#12854 = ORIENTED_EDGE ( 'NONE', *, *, #9782, .F. ) ;
#12855 = FACE_OUTER_BOUND ( 'NONE', #12214, .T. ) ;
#12856 = LINE ( 'NONE', #1624, #13420 ) ;
#12857 = DIRECTION ( 'NONE',  ( 0.000000000000000000, 0.000000000000000000, -1.000000000000000000 ) ) ;
#12858 = CARTESIAN_POINT ( 'NONE',  ( 15.40903463028482356, 46.52187500034139589, 47.42413220539093999 ) ) ;
#12859 = CARTESIAN_POINT ( 'NONE',  ( -30.81806926056963292, 31.55937500034139731, -42.41743335407647209 ) ) ;
#12860 = DIRECTION ( 'NONE',  ( -1.000000000000000000, 0.000000000000000000, -0.000000000000000000 ) ) ;
#12861 = AXIS2_PLACEMENT_3D ( 'NONE', #376, #3623, #15328 ) ;
#12862 = CARTESIAN_POINT ( 'NONE',  ( -40.34137639590981195, 48.12187500034139731, 29.30972558990012189 ) ) ;
#12863 = CARTESIAN_POINT ( 'NONE',  ( 0.000000000000000000, 267.0000000000000000, 0.000000000000000000 ) ) ;
#12864 = FACE_OUTER_BOUND ( 'NONE', #5741, .T. ) ;
#12865 = CARTESIAN_POINT ( 'NONE',  ( 9.574901606694759531E-15, 52.00000000000001421, -2.191293403013901163E-14 ) ) ;
#12866 = ORIENTED_EDGE ( 'NONE', *, *, #13116, .T. ) ;
#12867 =( BOUNDED_CURVE ( )  B_SPLINE_CURVE ( 2, ( #16233, #13647, #11002, #5774, #15905, #9843, #14895, #13487, #12323, #10919, #9592, #8503, #14719 ),
 .UNSPECIFIED., .F., .F. ) 
 B_SPLINE_CURVE_WITH_KNOTS ( ( 3, 2, 2, 2, 2, 2, 3 ),
 ( 0.6833333333333333481, 0.6866666666666666474, 0.6933333333333333570, 0.6999999999999999556, 0.7066666666666666652, 0.7133333333333333748, 0.7166666666666666741 ),
 .UNSPECIFIED. ) 
 CURVE ( )  GEOMETRIC_REPRESENTATION_ITEM ( )  RATIONAL_B_SPLINE_CURVE ( ( 0.9755282581475768211, 0.9755282581475768211, 1.000000000000000000, 0.9510565162951535312, 1.000000000000000000, 0.9510565162951535312, 1.000000000000000000, 0.9510565162951535312, 1.000000000000000000, 0.9510565162951535312, 1.000000000000000000, 0.9755282581475768211, 0.9755282581475768211 ) ) 
 REPRESENTATION_ITEM ( '' )  );
#12868 = CARTESIAN_POINT ( 'NONE',  ( 40.34137639590981195, 49.12187500034139731, -29.30972558990011834 ) ) ;
#12869 = ORIENTED_EDGE ( 'NONE', *, *, #320, .T. ) ;
#12870 = CARTESIAN_POINT ( 'NONE',  ( 0.000000000000000000, 245.0000000000000284, -47.99999999999999289 ) ) ;
#12871 = ORIENTED_EDGE ( 'NONE', *, *, #1637, .F. ) ;
#12872 = EDGE_LOOP ( 'NONE', ( #3814, #9199, #7405, #11584 ) ) ;
#12873 =( GEOMETRIC_REPRESENTATION_CONTEXT ( 3 ) GLOBAL_UNCERTAINTY_ASSIGNED_CONTEXT ( ( #15900 ) ) GLOBAL_UNIT_ASSIGNED_CONTEXT ( ( #12392, #9895, #2072 ) ) REPRESENTATION_CONTEXT ( 'NONE', 'WORKASPACE' ) );
#12874 = EDGE_CURVE ( 'NONE', #14188, #3621, #10365, .T. ) ;
#12875 = CARTESIAN_POINT ( 'NONE',  ( -2.547328955960238000E-13, 34.28125000068279604, 49.99999999999999289 ) ) ;
#12876 = CARTESIAN_POINT ( 'NONE',  ( -8.660254037844387298, 20.00000000000000355, 5.000000000000000000 ) ) ;
#12877 = CARTESIAN_POINT ( 'NONE',  ( 50.00000000000000000, 29.00000000000000000, -6.123233995736766085E-15 ) ) ;
#12878 = CARTESIAN_POINT ( 'NONE',  ( 15.45084971874736723, 25.40000000000000213, -47.55282581475768211 ) ) ;
#12879 = CARTESIAN_POINT ( 'NONE',  ( 15.45084971874736723, 33.18125000068279462, -47.55282581475768211 ) ) ;
#12880 = CARTESIAN_POINT ( 'NONE',  ( -50.00000000000000000, 31.78125000068279959, 0.000000000000000000 ) ) ;
#12881 = DIRECTION ( 'NONE',  ( -0.000000000000000000, 1.000000000000000000, -0.000000000000000000 ) ) ;
#12882 = CARTESIAN_POINT ( 'NONE',  ( 49.86468353125000164, 22.92187500034139802, -6.106662507704105588E-15 ) ) ;
#12883 = PLANE ( 'NONE',  #15498 ) ;
#12884 = CARTESIAN_POINT ( 'NONE',  ( -30.90169943749473802, 40.08125000068279320, 42.53254041760200721 ) ) ;
#12885 = CARTESIAN_POINT ( 'NONE',  ( 1.790468199911983804, 98.25246584726775723, 9.080892972013892006 ) ) ;
#12886 = VECTOR ( 'NONE', #4155, 1000.000000000000000 ) ;
#12887 = CARTESIAN_POINT ( 'NONE',  ( 15.45084971874737789, 24.60000000000000142, 47.55282581475767500 ) ) ;
#12888 =( LENGTH_UNIT ( ) NAMED_UNIT ( * ) SI_UNIT ( .MILLI., .METRE. ) );
#12889 = COLOUR_RGB ( '', 0.40784314, 0.44705882, 0.49803922) ;
#12890 = VERTEX_POINT ( 'NONE', #11689 ) ;
#12891 = CARTESIAN_POINT ( 'NONE',  ( -49.86468353124999453, 35.95937500034139589, 16.20201782572377525 ) ) ;
#12892 = VERTEX_POINT ( 'NONE', #10538 ) ;
#12893 = CARTESIAN_POINT ( 'NONE',  ( 40.45084971874737789, 42.80000000000000426, 29.38926261462365375 ) ) ;
#12894 = AXIS2_PLACEMENT_3D ( 'NONE', #6900, #1726, #10876 ) ;
#12895 = CARTESIAN_POINT ( 'NONE',  ( 0.5000000000000000000, 39.99999999999999289, 101.0000000000000000 ) ) ;
#12896 = CARTESIAN_POINT ( 'NONE',  ( -49.86468353124999453, 31.95937500034139944, 16.20201782572377525 ) ) ;
#12897 = VECTOR ( 'NONE', #11234, 1000.000000000000000 ) ;
#12898 = ORIENTED_EDGE ( 'NONE', *, *, #16428, .F. ) ;
#12899 = CARTESIAN_POINT ( 'NONE',  ( 8.446640517145639571E-15, 28.28125000068279959, 50.00000000000000000 ) ) ;
#12901 = ADVANCED_FACE ( 'NONE', ( #289 ), #367, .T. ) ;
#12900 = CARTESIAN_POINT ( 'NONE',  ( -6.186240466588083464, 38.88034870839190660, 92.94021688847078622 ) ) ;
#12902 = MECHANICAL_DESIGN_GEOMETRIC_PRESENTATION_REPRESENTATION (  '', ( #6543 ), #4676 ) ;
#12903 = CARTESIAN_POINT ( 'NONE',  ( 7.347880794884119933E-15, 52.00000000000000711, 60.00000000000000711 ) ) ;
#12904 = CARTESIAN_POINT ( 'NONE',  ( -30.81806926056963292, 35.62187500034140442, -42.41743335407646498 ) ) ;
#12905 = DIRECTION ( 'NONE',  ( 0.000000000000000000, 0.000000000000000000, -1.000000000000000000 ) ) ;
#12906 = CARTESIAN_POINT ( 'NONE',  ( -49.86468353124999453, 21.75937500034139305, -16.20201782572375393 ) ) ;
#12907 = LINE ( 'NONE', #258, #11078 ) ;
#12908 = CARTESIAN_POINT ( 'NONE',  ( 15.40903463028482356, 30.52187500034139589, 47.42413220539093999 ) ) ;
#12909 = CYLINDRICAL_SURFACE ( 'NONE', #3367, 50.00000000000000000 ) ;
#12910 = CLOSED_SHELL ( 'NONE', ( #16254, #6355, #3160, #11494, #15749, #3425, #13525, #11722, #15523, #10290, #12466, #11401, #406, #5731, #9297, #11989, #13412, #10090, #2134, #13267, #11951, #11190, #2234, #4391, #5490, #8749, #6773, #659, #10686, #7928, #16047, #2434, #3569, #1925, #7580, #15767, #4016, #503, #6987, #6430, #7780, #3723, #15701, #2009, #13646, #14032, #8663, #13165, #7437, #10981, #8252 ) ) ;
#12911 = CARTESIAN_POINT ( 'NONE',  ( 30.90169943749475578, 30.70000000000000284, 42.53254041760200010 ) ) ;
#12912 = CARTESIAN_POINT ( 'NONE',  ( -15.40903463028480580, 30.25937500034140015, 47.42413220539094709 ) ) ;
#12913 = AXIS2_PLACEMENT_3D ( 'NONE', #13649, #3351, #8260 ) ;
#12914 = CARTESIAN_POINT ( 'NONE',  ( -30.81806926056963292, 29.62187500034139376, -42.41743335407647209 ) ) ;
#12915 = AXIS2_PLACEMENT_3D ( 'NONE', #13380, #333, #14302 ) ;
#12916 = CIRCLE ( 'NONE', #10792, 17.50000000000000000 ) ;
#12917 = ORIENTED_EDGE ( 'NONE', *, *, #14334, .T. ) ;
#12918 = AXIS2_PLACEMENT_3D ( 'NONE', #10628, #13030, #1713 ) ;
#12919 = EDGE_CURVE ( 'NONE', #7079, #10200, #4299, .T. ) ;
#12920 = CARTESIAN_POINT ( 'NONE',  ( 15.40903463028481113, 37.25937500034140015, -47.42413220539094709 ) ) ;
#12921 = ORIENTED_EDGE ( 'NONE', *, *, #15235, .F. ) ;
#12922 = DIRECTION ( 'NONE',  ( 0.000000000000000000, -0.9848077530122080203, 0.1736481776669307198 ) ) ;
#12923 = CARTESIAN_POINT ( 'NONE',  ( 50.00000000000000711, 20.68125000068280173, 16.24598481164530739 ) ) ;
#12924 = EDGE_CURVE ( 'NONE', #4712, #7684, #8024, .T. ) ;
#12925 = CONICAL_SURFACE ( 'NONE', #2567, 100.0000000000000000, 0.1745329251994333364 ) ;
#12926 = CARTESIAN_POINT ( 'NONE',  ( -40.45084971874737789, 37.79999999999999716, -29.38926261462365730 ) ) ;
#12927 = AXIS2_PLACEMENT_3D ( 'NONE', #3564, #2385, #13689 ) ;
#12928 = CARTESIAN_POINT ( 'NONE',  ( -49.86468353125000164, 23.92187500034139447, 0.000000000000000000 ) ) ;
#12929 = CARTESIAN_POINT ( 'NONE',  ( -24.98849325795416121, 282.6608420050619088, 9.994246628976299007 ) ) ;
#12930 = CARTESIAN_POINT ( 'NONE',  ( -15.40903463028480580, 34.32187500034139305, 47.42413220539094709 ) ) ;
#12931 = CARTESIAN_POINT ( 'NONE',  ( 9.631387414534489405E-15, 44.35937500034140157, 52.43083105670540789 ) ) ;
#12932 = CARTESIAN_POINT ( 'NONE',  ( -49.99999999999999289, 25.68125000068279817, -16.24598481164531449 ) ) ;
#12933 = CARTESIAN_POINT ( 'NONE',  ( -15.40903463028480580, 20.32187500034139660, 47.42413220539094709 ) ) ;
#12934 = EDGE_CURVE ( 'NONE', #11147, #12980, #9455, .T. ) ;
#12935 = CARTESIAN_POINT ( 'NONE',  ( 49.99999999999999289, 20.88125000068279746, -16.24598481164532160 ) ) ;
#12936 = CARTESIAN_POINT ( 'NONE',  ( 40.34137639590981905, 48.72187500034139873, 29.30972558990010768 ) ) ;
#12937 = CARTESIAN_POINT ( 'NONE',  ( -3.210462471511496205E-15, 29.42187500034139092, -52.43083105670540789 ) ) ;
#12938 = AXIS2_PLACEMENT_3D ( 'NONE', #8223, #5982, #13289 ) ;
#12939 = VECTOR ( 'NONE', #2706, 999.9999999999998863 ) ;
#12940 = CARTESIAN_POINT ( 'NONE',  ( -24.78626291527393377, 40.00000000000000711, -5.650101528493794767 ) ) ;
#12941 = VERTEX_POINT ( 'NONE', #16311 ) ;
#12942 = CARTESIAN_POINT ( 'NONE',  ( -49.99999999999999289, 35.88125000068279746, 16.24598481164533226 ) ) ;
#12943 = ORIENTED_EDGE ( 'NONE', *, *, #11376, .T. ) ;
#12944 = DIRECTION ( 'NONE',  ( -0.000000000000000000, -1.000000000000000000, -0.000000000000000000 ) ) ;
#12945 = FACE_OUTER_BOUND ( 'NONE', #9566, .T. ) ;
#12946 = CARTESIAN_POINT ( 'NONE',  ( -15.11046079763414696, 14.35332166009617261, 101.3333374614808662 ) ) ;
#12947 = CARTESIAN_POINT ( 'NONE',  ( 5.000000000000000000, 99.58041009241404140, -7.580410092414002321 ) ) ;
#12948 = CARTESIAN_POINT ( 'NONE',  ( 30.81806926056964002, 22.55937500034139020, 42.41743335407647209 ) ) ;
#12949 = EDGE_CURVE ( 'NONE', #2250, #8059, #12373, .T. ) ;
#12950 = LINE ( 'NONE', #2328, #12653 ) ;
#12951 = CARTESIAN_POINT ( 'NONE',  ( -3.210462471511496205E-15, 39.42187500034139447, -52.43083105670540789 ) ) ;
#12952 = CYLINDRICAL_SURFACE ( 'NONE', #10745, 50.00000000000000000 ) ;
#12953 = CARTESIAN_POINT ( 'NONE',  ( 49.86468353124999453, 45.02187500034138878, -16.20201782572376459 ) ) ;
#12954 = DIRECTION ( 'NONE',  ( 0.000000000000000000, 1.000000000000000000, 0.000000000000000000 ) ) ;
#12955 = ORIENTED_EDGE ( 'NONE', *, *, #12100, .F. ) ;
#12956 = CARTESIAN_POINT ( 'NONE',  ( 30.81806926056964002, 20.55937500034139376, 42.41743335407647209 ) ) ;
#12957 = AXIS2_PLACEMENT_3D ( 'NONE', #10877, #14598, #5892 ) ;
#12958 = VERTEX_POINT ( 'NONE', #4947 ) ;
#12959 = CARTESIAN_POINT ( 'NONE',  ( -50.00000000000000000, 26.00000000000000355, 0.000000000000000000 ) ) ;
#12960 = ORIENTED_EDGE ( 'NONE', *, *, #1873, .T. ) ;
#12961 = ORIENTED_EDGE ( 'NONE', *, *, #915, .T. ) ;
#12962 = LINE ( 'NONE', #4154, #2586 ) ;
#12963 = PLANE ( 'NONE',  #7049 ) ;
#12964 = CARTESIAN_POINT ( 'NONE',  ( 5.000000000000000888, 91.24478243472064776, -8.497612305159609747 ) ) ;
#12965 = CARTESIAN_POINT ( 'NONE',  ( 49.99999999999999289, 23.10000000000000497, -16.24598481164532160 ) ) ;
#12966 = CARTESIAN_POINT ( 'NONE',  ( -15.40903463028481646, 45.45937500034139589, -47.42413220539093999 ) ) ;
#12967 = CARTESIAN_POINT ( 'NONE',  ( -30.27664397204038593, 40.00000000000000711, 26.14048258526057467 ) ) ;
#12968 = PLANE ( 'NONE',  #13774 ) ;
#12969 = CARTESIAN_POINT ( 'NONE',  ( 30.81806926056962936, 21.22187500034139518, -42.41743335407647209 ) ) ;
#12970 = CIRCLE ( 'NONE', #7923, 45.00000000000000000 ) ;
#12971 = DIRECTION ( 'NONE',  ( 0.7431448254773955764, -0.6691306063588567943, 0.000000000000000000 ) ) ;
#12972 = CARTESIAN_POINT ( 'NONE',  ( 9.657523855033129090E-15, 40.28125000068278894, 52.57311121191334990 ) ) ;
#12973 = DIRECTION ( 'NONE',  ( 1.000000000000000000, 0.000000000000000000, 0.000000000000000000 ) ) ;
#12974 = EDGE_CURVE ( 'NONE', #5249, #12890, #4572, .T. ) ;
#12975 = CARTESIAN_POINT ( 'NONE',  ( 40.45084971874737789, 46.58125000068280031, 29.38926261462365375 ) ) ;
#12976 = EDGE_CURVE ( 'NONE', #4332, #11447, #13566, .T. ) ;
#12977 = CARTESIAN_POINT ( 'NONE',  ( -30.27664397204056712, 25.00000000000000355, -26.14048258526036150 ) ) ;
#12978 = ORIENTED_EDGE ( 'NONE', *, *, #11943, .T. ) ;
#12979 = CARTESIAN_POINT ( 'NONE',  ( 30.81806926056962936, 39.15937500034139873, -42.41743335407647209 ) ) ;
#12980 = VERTEX_POINT ( 'NONE', #7182 ) ;
#12981 = CARTESIAN_POINT ( 'NONE',  ( 49.99999999999999289, 43.10000000000000142, -16.24598481164532160 ) ) ;
#12982 = DIRECTION ( 'NONE',  ( 0.000000000000000000, 1.000000000000000000, 0.000000000000000000 ) ) ;
#12983 = CARTESIAN_POINT ( 'NONE',  ( 49.86468353124999453, 22.95937500034139589, -16.20201782572376459 ) ) ;
#12984 = VERTEX_POINT ( 'NONE', #11334 ) ;
#12985 = DIRECTION ( 'NONE',  ( 0.000000000000000000, -1.000000000000000000, 0.000000000000000000 ) ) ;
#12986 = CARTESIAN_POINT ( 'NONE',  ( -17.36342088942478057, 24.75448731571099259, 94.04567196164467191 ) ) ;
#12987 = CARTESIAN_POINT ( 'NONE',  ( 0.000000000000000000, 242.0000000000000284, 0.000000000000000000 ) ) ;
#12988 = CARTESIAN_POINT ( 'NONE',  ( 40.34137639590981195, 29.12187500034139376, -29.30972558990011834 ) ) ;
#12989 = CARTESIAN_POINT ( 'NONE',  ( -9.500222237632405253, 22.00424054664139817, 101.0000000000000000 ) ) ;
#12990 = CARTESIAN_POINT ( 'NONE',  ( 15.18950378164810822, 13.79078835917772672, 96.37912034925916771 ) ) ;
#12991 = CARTESIAN_POINT ( 'NONE',  ( -46.73878613316165342, 20.00000000000001066, 17.37815620099909708 ) ) ;
#12992 = CARTESIAN_POINT ( 'NONE',  ( -40.34137639590981905, 31.72187500034139873, -29.30972558990011478 ) ) ;
#12993 = CARTESIAN_POINT ( 'NONE',  ( -20.00000000000000355, 287.0000000000000568, -7.499999999999999112 ) ) ;
#12994 = CONICAL_SURFACE ( 'NONE', #9020, 85.01963570546854498, 0.9599310885968793672 ) ;
#12995 = CARTESIAN_POINT ( 'NONE',  ( -15.45084971874736368, 34.39999999999999858, 47.55282581475768211 ) ) ;
#12996 = CARTESIAN_POINT ( 'NONE',  ( 49.86468353124999453, 30.95937500034139944, -16.20201782572376459 ) ) ;
#12997 = CARTESIAN_POINT ( 'NONE',  ( -49.86468353124999453, 28.02187500034139234, 16.20201782572377525 ) ) ;
#12998 = CARTESIAN_POINT ( 'NONE',  ( -20.00000000000114042, 286.6727470533917312, -7.500000000000000888 ) ) ;
#12999 = ORIENTED_EDGE ( 'NONE', *, *, #10006, .F. ) ;
#13000 = CARTESIAN_POINT ( 'NONE',  ( 9.631387414534489405E-15, 28.35937500034139447, 52.43083105670540789 ) ) ;
#13001 = ORIENTED_EDGE ( 'NONE', *, *, #800, .T. ) ;
#13002 = CARTESIAN_POINT ( 'NONE',  ( 29.34549410641264444, 282.0000000000000000, -12.17274705320872741 ) ) ;
#13003 = CARTESIAN_POINT ( 'NONE',  ( 30.81806926056964002, 46.55937500034139020, 42.41743335407647209 ) ) ;
#13004 = AXIS2_PLACEMENT_3D ( 'NONE', #8977, #5167, #10310 ) ;
#13005 = CARTESIAN_POINT ( 'NONE',  ( 9.395693774364776374, 21.00971865127324634, 101.0000000000000000 ) ) ;
#13006 = CARTESIAN_POINT ( 'NONE',  ( 27.49424662897629545, 282.6608420050619088, 7.488493257954154991 ) ) ;
#13007 = CARTESIAN_POINT ( 'NONE',  ( -30.00000000000000711, 282.0000000000000000, 12.50000000000000000 ) ) ;
#13008 = CARTESIAN_POINT ( 'NONE',  ( -30.81806926056962226, 38.22187500034139873, 42.41743335407647919 ) ) ;
#13009 = CARTESIAN_POINT ( 'NONE',  ( 49.86468353124999453, 32.95937500034138878, -16.20201782572376104 ) ) ;
#13010 = CYLINDRICAL_SURFACE ( 'NONE', #8114, 79.49773270518484480 ) ;
#13011 = ADVANCED_FACE ( 'NONE', ( #11177 ), #8573, .T. ) ;
#13012 = CARTESIAN_POINT ( 'NONE',  ( -30.90169943749473802, 38.29999999999999716, 42.53254041760200721 ) ) ;
#13013 = CARTESIAN_POINT ( 'NONE',  ( -40.45084971874737079, 21.98125000068279888, 29.38926261462367151 ) ) ;
#13014 = CARTESIAN_POINT ( 'NONE',  ( 30.81806926056962936, 45.22187500034139873, -42.41743335407647209 ) ) ;
#13015 = CARTESIAN_POINT ( 'NONE',  ( -30.81806926056963292, 25.62187500034139731, -42.41743335407647209 ) ) ;
#13016 = EDGE_CURVE ( 'NONE', #7399, #13988, #7253, .T. ) ;
#13017 = CARTESIAN_POINT ( 'NONE',  ( 49.86468353124999453, 48.95937500034140299, -16.20201782572376104 ) ) ;
#13018 = ORIENTED_EDGE ( 'NONE', *, *, #13590, .F. ) ;
#13019 = CARTESIAN_POINT ( 'NONE',  ( -50.00000000000000000, 39.78125000068279604, 0.000000000000000000 ) ) ;
#13020 = ORIENTED_EDGE ( 'NONE', *, *, #11376, .F. ) ;
#13021 = EDGE_CURVE ( 'NONE', #15674, #1275, #11001, .T. ) ;
#13022 = CARTESIAN_POINT ( 'NONE',  ( 1.022488062601840571E-14, 49.28125000068280315, -50.00000000000000000 ) ) ;
#13023 = DIRECTION ( 'NONE',  ( 0.000000000000000000, 0.000000000000000000, -1.000000000000000000 ) ) ;
#13024 = DIRECTION ( 'NONE',  ( 0.000000000000000000, 0.000000000000000000, -1.000000000000000000 ) ) ;
#13025 = CARTESIAN_POINT ( 'NONE',  ( 49.86468353125000164, 44.92187500034140157, -6.106662507704105588E-15 ) ) ;
#13026 = CARTESIAN_POINT ( 'NONE',  ( -15.40903463028480580, 24.25937500034139660, 47.42413220539094709 ) ) ;
#13027 = CARTESIAN_POINT ( 'NONE',  ( -6.725310538855818976, 29.22831317314782851, 101.0000000000000000 ) ) ;
#13028 = ADVANCED_FACE ( 'NONE', ( #6180 ), #9201, .T. ) ;
#13029 = CARTESIAN_POINT ( 'NONE',  ( 15.40903463028482356, 42.52187500034139589, 47.42413220539093999 ) ) ;
#13030 = DIRECTION ( 'NONE',  ( 0.000000000000000000, 0.000000000000000000, 1.000000000000000000 ) ) ;
#13031 = DIRECTION ( 'NONE',  ( -0.000000000000000000, -0.000000000000000000, 1.000000000000000000 ) ) ;
#13032 = CARTESIAN_POINT ( 'NONE',  ( -49.86468353125000164, 45.92187500034139447, 0.000000000000000000 ) ) ;
#13033 = CARTESIAN_POINT ( 'NONE',  ( 50.00000000000000000, 28.78125000068279959, -6.123233995736766085E-15 ) ) ;
#13034 = VERTEX_POINT ( 'NONE', #12321 ) ;
#13035 = CARTESIAN_POINT ( 'NONE',  ( 49.86468353125000164, 46.92187500034139447, -6.106662507704105588E-15 ) ) ;
#13036 = PRODUCT_DEFINITION_SHAPE ( 'NONE', 'NONE',  #16469 ) ;
#13037 = ORIENTED_EDGE ( 'NONE', *, *, #15336, .T. ) ;
#13038 = CARTESIAN_POINT ( 'NONE',  ( -49.99999999999999289, 26.10000000000000142, 16.24598481164533226 ) ) ;
#13039 = ORIENTED_EDGE ( 'NONE', *, *, #13228, .F. ) ;
#13040 = ORIENTED_EDGE ( 'NONE', *, *, #2345, .F. ) ;
#13041 = LINE ( 'NONE', #11785, #410 ) ;
#13042 = DIRECTION ( 'NONE',  ( 0.000000000000000000, 1.000000000000000000, 0.000000000000000000 ) ) ;
#13043 = CARTESIAN_POINT ( 'NONE',  ( 0.000000000000000000, 0.000000000000000000, 100.0000000000000000 ) ) ;
#13044 = CARTESIAN_POINT ( 'NONE',  ( 15.45084971874737789, 26.60000000000000142, 47.55282581475767500 ) ) ;
#13045 = CARTESIAN_POINT ( 'NONE',  ( -49.86468353125000164, 45.85937500034140157, 0.000000000000000000 ) ) ;
#13046 = CARTESIAN_POINT ( 'NONE',  ( -30.90169943749473447, 26.08125000068279320, 42.53254041760200721 ) ) ;
#13047 = CARTESIAN_POINT ( 'NONE',  ( -19.48557158514997312, 33.74999999999982236, 101.0000000000000000 ) ) ;
#13048 = ADVANCED_FACE ( 'NONE', ( #14974 ), #10257, .T. ) ;
#13049 = LINE ( 'NONE', #12125, #1503 ) ;
#13050 = SURFACE_STYLE_USAGE ( .BOTH. , #316 ) ;
#13051 = DIRECTION ( 'NONE',  ( 0.000000000000000000, 0.000000000000000000, 1.000000000000000000 ) ) ;
#13052 = CARTESIAN_POINT ( 'NONE',  ( 49.99999999999999289, 42.88125000068278325, -16.24598481164532160 ) ) ;
#13053 = CARTESIAN_POINT ( 'NONE',  ( 5.000000000000000000, 96.75198296766781425, 7.580410092413965017 ) ) ;
#13054 = CARTESIAN_POINT ( 'NONE',  ( 7.500000000000000000, 25.00000000000000355, -39.29058411375427795 ) ) ;
#13055 = DIRECTION ( 'NONE',  ( 0.9945218953682730678, 0.1045284632676572317, 0.000000000000000000 ) ) ;
#13056 = ORIENTED_EDGE ( 'NONE', *, *, #5053, .F. ) ;
#13057 = CARTESIAN_POINT ( 'NONE',  ( 15.40903463028482356, 38.45937500034139589, 47.42413220539093999 ) ) ;
#13058 = ORIENTED_EDGE ( 'NONE', *, *, #13116, .F. ) ;
#13059 = EDGE_LOOP ( 'NONE', ( #2671, #15856, #2108, #5798 ) ) ;
#13060 = CARTESIAN_POINT ( 'NONE',  ( -49.99999999999999289, 47.88125000068280457, 16.24598481164533226 ) ) ;
#13061 = DIRECTION ( 'NONE',  ( -0.000000000000000000, 1.000000000000000000, -0.000000000000000000 ) ) ;
#13062 = CARTESIAN_POINT ( 'NONE',  ( 9.631387414534489405E-15, 20.35937500034139092, 52.43083105670540789 ) ) ;
#13063 = ORIENTED_EDGE ( 'NONE', *, *, #8930, .F. ) ;
#13064 = EDGE_CURVE ( 'NONE', #14671, #8593, #8501, .T. ) ;
#13065 = LINE ( 'NONE', #6766, #5747 ) ;
#13066 = LINE ( 'NONE', #13142, #13680 ) ;
#13067 = DIRECTION ( 'NONE',  ( -0.000000000000000000, -1.000000000000000000, -0.000000000000000000 ) ) ;
#13068 = CARTESIAN_POINT ( 'NONE',  ( -49.86468353125000164, 25.92187500034139802, 0.000000000000000000 ) ) ;
#13069 =( BOUNDED_CURVE ( )  B_SPLINE_CURVE ( 2, ( #5922, #5671, #10902, #14792, #8559, #8486, #7169, #13552, #9498, #16140, #9651, #15799, #14703 ),
 .UNSPECIFIED., .F., .T. ) 
 B_SPLINE_CURVE_WITH_KNOTS ( ( 3, 2, 2, 2, 2, 2, 3 ),
 ( 0.3500000000000000333, 0.3533333333333333326, 0.3599999999999999867, 0.3666666666666666408, 0.3733333333333333504, 0.3800000000000000044, 0.3833333333333333592 ),
 .UNSPECIFIED. ) 
 CURVE ( )  GEOMETRIC_REPRESENTATION_ITEM ( )  RATIONAL_B_SPLINE_CURVE ( ( 0.9755282581475768211, 0.9755282581475770431, 1.000000000000000000, 0.9510565162951535312, 1.000000000000000000, 0.9510565162951535312, 1.000000000000000000, 0.9510565162951535312, 1.000000000000000000, 0.9510565162951535312, 1.000000000000000000, 0.9755282581475765991, 0.9755282581475768211 ) ) 
 REPRESENTATION_ITEM ( '' )  );
#13070 = CARTESIAN_POINT ( 'NONE',  ( -7.919222016226752814, 37.33250428222964246, -50.00000000000000711 ) ) ;
#13071 = CARTESIAN_POINT ( 'NONE',  ( -46.25745152662948811, 20.00000000000000355, 18.62156331808021648 ) ) ;
#13072 = CARTESIAN_POINT ( 'NONE',  ( 40.34137639590981195, 31.12187500034139731, -29.30972558990011834 ) ) ;
#13073 = CARTESIAN_POINT ( 'NONE',  ( -8.477241335952138357, 18.18301270189218855, 101.0000000000000000 ) ) ;
#13074 = CARTESIAN_POINT ( 'NONE',  ( -30.90169943749473802, 32.30000000000000426, 42.53254041760200721 ) ) ;
#13075 = CARTESIAN_POINT ( 'NONE',  ( -40.34137639590981195, 30.05937500034139731, 29.30972558990012189 ) ) ;
#13076 = DIRECTION ( 'NONE',  ( 0.000000000000000000, -1.000000000000000000, 0.000000000000000000 ) ) ;
#13077 = ORIENTED_EDGE ( 'NONE', *, *, #6067, .T. ) ;
#13078 = VECTOR ( 'NONE', #4142, 999.9999999999998863 ) ;
#13079 = CARTESIAN_POINT ( 'NONE',  ( -15.40903463028480580, 30.25937500034140015, 47.42413220539094709 ) ) ;
#13080 = ORIENTED_EDGE ( 'NONE', *, *, #1432, .F. ) ;
#13081 = DIRECTION ( 'NONE',  ( -0.000000000000000000, 0.000000000000000000, -1.000000000000000000 ) ) ;
#13082 = CARTESIAN_POINT ( 'NONE',  ( -49.86468353124999453, 39.75937500034139305, -16.20201782572375393 ) ) ;
#13083 = CARTESIAN_POINT ( 'NONE',  ( -7.580410092413979228, 99.32916037694960210, -5.000000000000000000 ) ) ;
#13084 = CARTESIAN_POINT ( 'NONE',  ( 25.03223043949678939, 286.3455096218834797, 2.564460878999445193 ) ) ;
#13085 = CARTESIAN_POINT ( 'NONE',  ( -24.81239020281865137, 286.7275190727449967, 7.312390202818650486 ) ) ;
#13086 = CARTESIAN_POINT ( 'NONE',  ( -15.40903463028481646, 33.52187500034140299, -47.42413220539093999 ) ) ;
#13087 = CARTESIAN_POINT ( 'NONE',  ( -40.34137639590981195, 38.05937500034139731, 29.30972558990012189 ) ) ;
#13088 = CARTESIAN_POINT ( 'NONE',  ( 17.28626291527369929, 25.00000000000000355, -18.64048258526063151 ) ) ;
#13089 = CARTESIAN_POINT ( 'NONE',  ( -30.90169943749473802, 42.30000000000000426, 42.53254041760200721 ) ) ;
#13090 = AXIS2_PLACEMENT_3D ( 'NONE', #9268, #3185, #14562 ) ;
#13091 = CARTESIAN_POINT ( 'NONE',  ( 30.81806926056962936, 49.15937500034138452, -42.41743335407647209 ) ) ;
#13092 = CARTESIAN_POINT ( 'NONE',  ( 49.86468353124999453, 43.02187500034138878, -16.20201782572376459 ) ) ;
#13093 = EDGE_CURVE ( 'NONE', #14942, #7759, #6279, .T. ) ;
#13094 = CARTESIAN_POINT ( 'NONE',  ( 15.40903463028481113, 29.32187500034139660, -47.42413220539094709 ) ) ;
#13095 = ADVANCED_FACE ( 'NONE', ( #2093 ), #12243, .F. ) ;
#13096 = CARTESIAN_POINT ( 'NONE',  ( -49.99999999999999289, 27.68125000068279462, -16.24598481164531449 ) ) ;
#13097 = ORIENTED_EDGE ( 'NONE', *, *, #2891, .F. ) ;
#13098 = CARTESIAN_POINT ( 'NONE',  ( -15.45084971874736368, 30.18125000068280173, 47.55282581475768211 ) ) ;
#13099 = AXIS2_PLACEMENT_3D ( 'NONE', #14116, #1572, #15370 ) ;
#13100 = EDGE_LOOP ( 'NONE', ( #6614, #9283 ) ) ;
#13101 = FACE_OUTER_BOUND ( 'NONE', #9218, .T. ) ;
#13102 = CARTESIAN_POINT ( 'NONE',  ( -5.179451399590974781, 14.52044592729175321, 101.0000000000000000 ) ) ;
#13103 = CARTESIAN_POINT ( 'NONE',  ( -49.86468353125000164, 49.92187500034140157, 0.000000000000000000 ) ) ;
#13104 = CARTESIAN_POINT ( 'NONE',  ( -49.86468353124999453, 27.75937500034139660, -16.20201782572375393 ) ) ;
#13105 = EDGE_CURVE ( 'NONE', #8121, #13641, #7246, .T. ) ;
#13106 = LINE ( 'NONE', #1710, #15782 ) ;
#13107 = CARTESIAN_POINT ( 'NONE',  ( -40.34137639590981195, 40.12187500034139731, 29.30972558990012189 ) ) ;
#13108 = VECTOR ( 'NONE', #13211, 1000.000000000000000 ) ;
#13109 = CARTESIAN_POINT ( 'NONE',  ( 40.34137639590981905, 44.72187500034139163, 29.30972558990010768 ) ) ;
#13110 = CARTESIAN_POINT ( 'NONE',  ( -30.90169943749473447, 46.08125000068279320, 42.53254041760200721 ) ) ;
#13111 = EDGE_LOOP ( 'NONE', ( #12834, #15597, #12141, #15324 ) ) ;
#13112 = CARTESIAN_POINT ( 'NONE',  ( 49.86468353124999453, 20.95937500034138878, -16.20201782572376459 ) ) ;
#13113 = ORIENTED_EDGE ( 'NONE', *, *, #8876, .F. ) ;
#13114 = DIRECTION ( 'NONE',  ( 0.000000000000000000, 1.000000000000000000, 0.000000000000000000 ) ) ;
#13115 = ORIENTED_EDGE ( 'NONE', *, *, #8637, .F. ) ;
#13116 = EDGE_CURVE ( 'NONE', #14108, #7047, #5109, .T. ) ;
#13117 = CARTESIAN_POINT ( 'NONE',  ( -49.99999999999999289, 43.88125000068279746, 16.24598481164533226 ) ) ;
#13118 = LINE ( 'NONE', #13280, #11825 ) ;
#13119 = CARTESIAN_POINT ( 'NONE',  ( -50.00000000000000000, 49.89062500034140157, 0.000000000000000000 ) ) ;
#13120 = CARTESIAN_POINT ( 'NONE',  ( -40.45084971874737079, 26.20000000000000284, 29.38926261462367151 ) ) ;
#13121 = CARTESIAN_POINT ( 'NONE',  ( 15.40903463028482356, 46.45937500034139589, 47.42413220539093999 ) ) ;
#13122 = PLANE ( 'NONE',  #9930 ) ;
#13123 = LINE ( 'NONE', #5413, #14298 ) ;
#13124 = DIRECTION ( 'NONE',  ( 0.000000000000000000, 0.000000000000000000, -1.000000000000000000 ) ) ;
#13125 = EDGE_CURVE ( 'NONE', #4476, #12134, #11654, .T. ) ;
#13126 = CARTESIAN_POINT ( 'NONE',  ( -7.394441145214675437, 28.48516834767043093, 101.0000000000000000 ) ) ;
#13127 = CARTESIAN_POINT ( 'NONE',  ( 40.45084971874737079, 36.98125000068279888, -29.38926261462366440 ) ) ;
#13128 = CARTESIAN_POINT ( 'NONE',  ( -3.111920190527341144E-15, 43.50000000000000711, -50.00000000000000000 ) ) ;
#13129 = EDGE_CURVE ( 'NONE', #1977, #14690, #9158, .T. ) ;
#13130 = CARTESIAN_POINT ( 'NONE',  ( 7.919222016226940219, 23.22999571913595673, -49.99999999999996447 ) ) ;
#13131 = DIRECTION ( 'NONE',  ( -0.000000000000000000, -1.000000000000000000, -0.000000000000000000 ) ) ;
#13132 = VERTEX_POINT ( 'NONE', #12899 ) ;
#13133 = AXIS2_PLACEMENT_3D ( 'NONE', #1370, #6383, #11366 ) ;
#13134 = CARTESIAN_POINT ( 'NONE',  ( 40.34137639590981195, 37.05937500034139731, -29.30972558990011834 ) ) ;
#13135 = ORIENTED_EDGE ( 'NONE', *, *, #1, .T. ) ;
#13136 = EDGE_LOOP ( 'NONE', ( #13263, #9818, #2856, #9341 ) ) ;
#13137 = CARTESIAN_POINT ( 'NONE',  ( 0.000000000000000000, 217.0000000000000284, 0.000000000000000000 ) ) ;
#13138 = DIRECTION ( 'NONE',  ( 1.000000000000000000, 0.000000000000000000, 0.000000000000000000 ) ) ;
#13139 = CARTESIAN_POINT ( 'NONE',  ( 49.86468353125000164, 24.85937500034139802, -6.106662507704105588E-15 ) ) ;
#13140 = ORIENTED_EDGE ( 'NONE', *, *, #13214, .T. ) ;
#13141 = LINE ( 'NONE', #10582, #7608 ) ;
#13142 = CARTESIAN_POINT ( 'NONE',  ( -13.33959974903384627, 33.83821319854129683, 101.0000000000000000 ) ) ;
#13143 = VECTOR ( 'NONE', #8357, 1000.000000000000000 ) ;
#13144 = DIRECTION ( 'NONE',  ( -0.000000000000000000, 1.000000000000000000, -0.000000000000000000 ) ) ;
#13145 = CARTESIAN_POINT ( 'NONE',  ( -30.81806926056963292, 27.62187500034139731, -42.41743335407646498 ) ) ;
#13146 = PRESENTATION_LAYER_ASSIGNMENT (  '', '', ( #4121 ) ) ;
#13147 = DIRECTION ( 'NONE',  ( 0.000000000000000000, -1.000000000000000000, 0.000000000000000000 ) ) ;
#13148 = CARTESIAN_POINT ( 'NONE',  ( -45.11452830843730766, 20.00000000000000711, 21.24066852005664430 ) ) ;
#13149 = DIRECTION ( 'NONE',  ( 0.000000000000000000, 0.000000000000000000, -1.000000000000000000 ) ) ;
#13150 = EDGE_CURVE ( 'NONE', #10026, #4982, #2820, .T. ) ;
#13151 = CARTESIAN_POINT ( 'NONE',  ( -15.40903463028481646, 27.52187500034139944, -47.42413220539093999 ) ) ;
#13152 = CARTESIAN_POINT ( 'NONE',  ( 49.99999999999999289, 37.10000000000000142, -16.24598481164532160 ) ) ;
#13153 = CARTESIAN_POINT ( 'NONE',  ( -49.86468353125000164, 29.85937500034139802, 0.000000000000000000 ) ) ;
#13154 = CARTESIAN_POINT ( 'NONE',  ( 7.513064459987437071E-14, 42.28125000068280315, 50.00000000000000000 ) ) ;
#13155 = EDGE_LOOP ( 'NONE', ( #11193, #667, #16325, #3389, #6425, #9053, #6215, #4077, #2066, #11536, #2436, #10179, #13056, #10853, #15654, #1415, #15112, #10301, #13319, #513, #8884, #10726, #11966, #5202 ) ) ;
#13156 = VECTOR ( 'NONE', #8291, 1000.000000000000000 ) ;
#13157 = CARTESIAN_POINT ( 'NONE',  ( -49.86468353125000164, 29.85937500034139802, 0.000000000000000000 ) ) ;
#13158 = ORIENTED_EDGE ( 'NONE', *, *, #8132, .F. ) ;
#13159 = MECHANICAL_DESIGN_GEOMETRIC_PRESENTATION_REPRESENTATION (  '', ( #3875 ), #9178 ) ;
#13160 = PLANE ( 'NONE',  #13436 ) ;
#13162 =( BOUNDED_CURVE ( )  B_SPLINE_CURVE ( 3, ( #5028, #11559, #1084, #11330 ),
 .UNSPECIFIED., .F., .F. ) 
 B_SPLINE_CURVE_WITH_KNOTS ( ( 4, 4 ),
 ( 4.712388980384689674, 4.901005366560093890 ),
 .UNSPECIFIED. ) 
 CURVE ( )  GEOMETRIC_REPRESENTATION_ITEM ( )  RATIONAL_B_SPLINE_CURVE ( ( 1.000000000000000000, 0.9970375182503885547, 0.9970375182503885547, 1.000000000000000000 ) ) 
 REPRESENTATION_ITEM ( '' )  );
#13161 = CARTESIAN_POINT ( 'NONE',  ( -30.81806926056962226, 44.15937500034139163, 42.41743335407647919 ) ) ;
#13163 = CARTESIAN_POINT ( 'NONE',  ( 1.671572875253809487, 242.8284271247462129, 49.99999999999999289 ) ) ;
#13164 = CARTESIAN_POINT ( 'NONE',  ( 30.00000000000000355, 282.0000000000000000, 12.50000000000000178 ) ) ;
#13165 = ADVANCED_FACE ( 'NONE', ( #6507 ), #14215, .T. ) ;
#13166 = CARTESIAN_POINT ( 'NONE',  ( -21.32168401022832782, 284.4942466288906076, 8.160842005119160802 ) ) ;
#13167 = EDGE_CURVE ( 'NONE', #14690, #7640, #12654, .T. ) ;
#13168 = CARTESIAN_POINT ( 'NONE',  ( 49.86468353125001585, 36.82187500034140015, 16.20201782572375038 ) ) ;
#13169 = CARTESIAN_POINT ( 'NONE',  ( 40.34137639590981905, 38.65937500034139873, 29.30972558990010768 ) ) ;
#13170 = VECTOR ( 'NONE', #3127, 1000.000000000000000 ) ;
#13171 = AXIS2_PLACEMENT_3D ( 'NONE', #11976, #3083, #8160 ) ;
#13172 = FACE_OUTER_BOUND ( 'NONE', #13136, .T. ) ;
#13173 = AXIS2_PLACEMENT_3D ( 'NONE', #9080, #5358, #11655 ) ;
#13174 = CARTESIAN_POINT ( 'NONE',  ( 15.45084971874736723, 39.40000000000000568, -47.55282581475768211 ) ) ;
#13175 = CARTESIAN_POINT ( 'NONE',  ( -3.219174618344376363E-15, 21.28125000068279959, -52.57311121191334990 ) ) ;
#13176 = CARTESIAN_POINT ( 'NONE',  ( -49.86468353125000164, 41.92187500034139447, 0.000000000000000000 ) ) ;
#13177 = PRESENTATION_LAYER_ASSIGNMENT (  '', '', ( #3346 ) ) ;
#13178 = CARTESIAN_POINT ( 'NONE',  ( 40.34137639590981195, 25.12187500034139376, -29.30972558990011834 ) ) ;
#13179 = DIRECTION ( 'NONE',  ( -0.000000000000000000, -1.000000000000000000, -0.000000000000000000 ) ) ;
#13180 = CLOSED_SHELL ( 'NONE', ( #12079, #11872, #14357, #10861, #12416, #2871, #4696, #16117, #16345, #16071, #2561, #14865, #11605, #13973, #16172, #12623, #14820, #4113, #15286, #15987, #415, #11779, #2135, #8968 ) ) ;
#13181 = ORIENTED_EDGE ( 'NONE', *, *, #10077, .F. ) ;
#13182 = AXIS2_PLACEMENT_3D ( 'NONE', #1593, #11735, #337 ) ;
#13183 = VECTOR ( 'NONE', #6099, 1000.000000000000000 ) ;
#13185 = CARTESIAN_POINT ( 'NONE',  ( -30.90169943749473802, 32.08125000068280031, 42.53254041760200721 ) ) ;
#13184 = VECTOR ( 'NONE', #12922, 1000.000000000000000 ) ;
#13186 = ORIENTED_EDGE ( 'NONE', *, *, #13339, .T. ) ;
#13187 = PLANE ( 'NONE',  #6523 ) ;
#13188 = CARTESIAN_POINT ( 'NONE',  ( 2.600676159226420495E-13, 33.28125000068279604, -49.99999999999999289 ) ) ;
#13189 = CARTESIAN_POINT ( 'NONE',  ( -49.86468353124999453, 49.82187500034139305, -16.20201782572375393 ) ) ;
#13190 = CARTESIAN_POINT ( 'NONE',  ( -3.210462471511496205E-15, 25.35937500034139802, -52.43083105670540789 ) ) ;
#13191 = DIRECTION ( 'NONE',  ( 6.938893903907231459E-18, -1.000000000000000000, -5.551115123125782702E-17 ) ) ;
#13192 = CARTESIAN_POINT ( 'NONE',  ( -15.40903463028480580, 40.32187500034140015, 47.42413220539094709 ) ) ;
#13193 = APPLICATION_PROTOCOL_DEFINITION ( 'draft international standard', 'automotive_design', 1998, #12378 ) ;
#13194 = VECTOR ( 'NONE', #4931, 1000.000000000000000 ) ;
#13195 = VECTOR ( 'NONE', #13299, 1000.000000000000000 ) ;
#13196 = CARTESIAN_POINT ( 'NONE',  ( -49.86468353124999453, 47.82187500034140015, -16.20201782572375393 ) ) ;
#13197 = CARTESIAN_POINT ( 'NONE',  ( -7.919222016226816763, 45.33250428222963535, -49.99999999999999289 ) ) ;
#13198 = EDGE_LOOP ( 'NONE', ( #7903, #3899, #8548, #1061 ) ) ;
#13199 = CARTESIAN_POINT ( 'NONE',  ( 40.34137639590981195, 45.12187500034139731, -29.30972558990011834 ) ) ;
#13200 = ORIENTED_EDGE ( 'NONE', *, *, #3497, .T. ) ;
#13201 = ORIENTED_EDGE ( 'NONE', *, *, #1229, .F. ) ;
#13202 = AXIS2_PLACEMENT_3D ( 'NONE', #7006, #7335, #4433 ) ;
#13203 = DIRECTION ( 'NONE',  ( -0.000000000000000000, -0.7071067811865487940, -0.7071067811865463515 ) ) ;
#13204 = DIRECTION ( 'NONE',  ( 0.000000000000000000, 0.000000000000000000, 1.000000000000000000 ) ) ;
#13205 = FACE_OUTER_BOUND ( 'NONE', #9605, .T. ) ;
#13206 = CARTESIAN_POINT ( 'NONE',  ( -40.45084971874737079, 24.20000000000000284, 29.38926261462367151 ) ) ;
#13207 = CARTESIAN_POINT ( 'NONE',  ( 49.86468353125000164, 46.85937500034139447, -6.106662507704105588E-15 ) ) ;
#13208 = CARTESIAN_POINT ( 'NONE',  ( -1.240322475938754499E-13, 38.50000000000000711, 50.00000000000000000 ) ) ;
#13209 = CARTESIAN_POINT ( 'NONE',  ( -2.547328955960238000E-13, 24.28125000068279604, 49.99999999999999289 ) ) ;
#13210 = DIRECTION ( 'NONE',  ( -0.000000000000000000, 1.000000000000000000, -0.000000000000000000 ) ) ;
#13211 = DIRECTION ( 'NONE',  ( -0.000000000000000000, 1.000000000000000000, -0.000000000000000000 ) ) ;
#13212 = CARTESIAN_POINT ( 'NONE',  ( -40.45084971874737789, 33.58125000068280031, -29.38926261462365730 ) ) ;
#13213 = DIRECTION ( 'NONE',  ( -0.7431448254773861395, -0.6691306063588672304, 0.000000000000000000 ) ) ;
#13214 = EDGE_CURVE ( 'NONE', #15423, #3157, #7908, .T. ) ;
#13215 = DIRECTION ( 'NONE',  ( 0.000000000000000000, 0.000000000000000000, 1.000000000000000000 ) ) ;
#13216 = DIRECTION ( 'NONE',  ( 0.000000000000000000, 1.000000000000000000, 0.000000000000000000 ) ) ;
#13217 = EDGE_LOOP ( 'NONE', ( #14340, #12292, #8605, #9572 ) ) ;
#13218 = CARTESIAN_POINT ( 'NONE',  ( -49.86468353125000164, 29.85937500034139802, 0.000000000000000000 ) ) ;
#13219 = EDGE_LOOP ( 'NONE', ( #11035, #7642, #719, #14860 ) ) ;
#13220 = ORIENTED_EDGE ( 'NONE', *, *, #8988, .T. ) ;
#13221 = EDGE_CURVE ( 'NONE', #4340, #14214, #2765, .T. ) ;
#13222 = EDGE_CURVE ( 'NONE', #13787, #10383, #5498, .T. ) ;
#13223 = PLANE ( 'NONE',  #10498 ) ;
#13224 = CARTESIAN_POINT ( 'NONE',  ( 12.67046914267482016, 34.58135802401886139, 101.0000000000000000 ) ) ;
#13225 = CARTESIAN_POINT ( 'NONE',  ( -49.86468353125000164, 19.85937500034139447, 0.000000000000000000 ) ) ;
#13226 = ORIENTED_EDGE ( 'NONE', *, *, #6218, .T. ) ;
#13227 = VECTOR ( 'NONE', #12619, 1000.000000000000000 ) ;
#13228 = EDGE_CURVE ( 'NONE', #4896, #6137, #11798, .T. ) ;
#13229 = CARTESIAN_POINT ( 'NONE',  ( -40.45084971874737789, 47.80000000000000426, -29.38926261462365730 ) ) ;
#13230 = CARTESIAN_POINT ( 'NONE',  ( -3.111920190527341144E-15, 35.50000000000000000, -50.00000000000000000 ) ) ;
#13231 = APPLICATION_CONTEXT ( 'automotive_design' ) ;
#13232 = DIRECTION ( 'NONE',  ( -1.000000000000000000, 6.938893903907222461E-16, 0.000000000000000000 ) ) ;
#13233 = LINE ( 'NONE', #16215, #479 ) ;
#13234 = CARTESIAN_POINT ( 'NONE',  ( -15.45084971874736368, 38.18125000068280173, 47.55282581475768211 ) ) ;
#13235 = CARTESIAN_POINT ( 'NONE',  ( 49.99999999999999289, 47.10000000000000142, -16.24598481164532160 ) ) ;
#13236 = CARTESIAN_POINT ( 'NONE',  ( 0.000000000000000000, 20.00000000000000355, 0.000000000000000000 ) ) ;
#13237 = CARTESIAN_POINT ( 'NONE',  ( -15.40903463028481646, 23.52187500034139944, -47.42413220539093999 ) ) ;
#13238 = CARTESIAN_POINT ( 'NONE',  ( 2.600676159226420495E-13, 21.50000000000000000, -49.99999999999999289 ) ) ;
#13239 = CARTESIAN_POINT ( 'NONE',  ( -40.45084971874737079, 32.20000000000000284, 29.38926261462367151 ) ) ;
#13240 = CARTESIAN_POINT ( 'NONE',  ( -40.34137639590981905, 27.65937500034139873, -29.30972558990011478 ) ) ;
#13241 = CARTESIAN_POINT ( 'NONE',  ( 37.77664397204061686, 40.00000000000000711, 13.15010152849349900 ) ) ;
#13242 = VERTEX_POINT ( 'NONE', #173 ) ;
#13243 = CARTESIAN_POINT ( 'NONE',  ( 30.81806926056962936, 31.15937500034139163, -42.41743335407646498 ) ) ;
#13244 = ORIENTED_EDGE ( 'NONE', *, *, #577, .F. ) ;
#13245 = CARTESIAN_POINT ( 'NONE',  ( -7.581784256837357461, 125.2766624725656897, 36.10508959731173917 ) ) ;
#13246 = CARTESIAN_POINT ( 'NONE',  ( 49.86468353124999453, 40.95937500034140299, -16.20201782572376459 ) ) ;
#13247 = CARTESIAN_POINT ( 'NONE',  ( 29.50911996093861234, 282.0000000000000000, 12.00911996093781653 ) ) ;
#13248 = CARTESIAN_POINT ( 'NONE',  ( -29.50911996093452672, 282.0000000000000000, 12.00911996094094292 ) ) ;
#13249 = CARTESIAN_POINT ( 'NONE',  ( -15.40903463028481646, 31.52187500034139944, -47.42413220539093999 ) ) ;
#13250 = CARTESIAN_POINT ( 'NONE',  ( 40.34137639590981195, 39.05937500034140442, -29.30972558990011834 ) ) ;
#13251 = FACE_OUTER_BOUND ( 'NONE', #11896, .T. ) ;
#13252 = CARTESIAN_POINT ( 'NONE',  ( 15.40903463028481113, 29.32187500034139660, -47.42413220539094709 ) ) ;
#13253 = CARTESIAN_POINT ( 'NONE',  ( -50.00000000000000000, 42.00000000000000000, 0.000000000000000000 ) ) ;
#13254 = CARTESIAN_POINT ( 'NONE',  ( 50.00000000000000711, 20.68125000068280173, 16.24598481164530739 ) ) ;
#13255 = CARTESIAN_POINT ( 'NONE',  ( 40.34137639590981195, 47.12187500034140442, -29.30972558990011834 ) ) ;
#13256 = CARTESIAN_POINT ( 'NONE',  ( -30.81806926056963292, 23.62187500034139731, -42.41743335407647209 ) ) ;
#13258 = EDGE_LOOP ( 'NONE', ( #5660, #16104, #14777, #3722 ) ) ;
#13257 =( BOUNDED_CURVE ( )  B_SPLINE_CURVE ( 3, ( #9069, #12885, #15374, #13053 ),
 .UNSPECIFIED., .F., .T. ) 
 B_SPLINE_CURVE_WITH_KNOTS ( ( 4, 4 ),
 ( 3.141592653589793116, 3.724683441357936609 ),
 .UNSPECIFIED. ) 
 CURVE ( )  GEOMETRIC_REPRESENTATION_ITEM ( )  RATIONAL_B_SPLINE_CURVE ( ( 1.000000000000000000, 0.9718672150731670900, 0.9718672150731670900, 1.000000000000000000 ) ) 
 REPRESENTATION_ITEM ( '' )  );
#13259 = TOROIDAL_SURFACE ( 'NONE', #3971, 7.732050807568878525, 2.000000000000000000 ) ;
#13260 = CARTESIAN_POINT ( 'NONE',  ( -30.81806926056962226, 46.15937500034139873, 42.41743335407647209 ) ) ;
#13261 = ORIENTED_EDGE ( 'NONE', *, *, #11209, .F. ) ;
#13262 = CARTESIAN_POINT ( 'NONE',  ( 9.657523855033129090E-15, 30.28125000068279604, 52.57311121191334990 ) ) ;
#13263 = ORIENTED_EDGE ( 'NONE', *, *, #14177, .T. ) ;
#13264 = CARTESIAN_POINT ( 'NONE',  ( 7.977241335952203194, 17.31698729810786475, 101.0000000000000000 ) ) ;
#13265 = CARTESIAN_POINT ( 'NONE',  ( 50.00000000000000711, 32.68125000068279462, 16.24598481164530739 ) ) ;
#13266 = CARTESIAN_POINT ( 'NONE',  ( -49.86468353124999453, 38.02187500034139589, 16.20201782572377169 ) ) ;
#13267 = ADVANCED_FACE ( 'NONE', ( #5278 ), #10329, .F. ) ;
#13268 = CARTESIAN_POINT ( 'NONE',  ( -15.40903463028481646, 23.45937500034139944, -47.42413220539093999 ) ) ;
#13269 = PLANE ( 'NONE',  #13421 ) ;
#13270 = VECTOR ( 'NONE', #2403, 1000.000000000000000 ) ;
#13271 = CONTEXT_DEPENDENT_SHAPE_REPRESENTATION ( #16308, #4008 ) ;
#13272 = CARTESIAN_POINT ( 'NONE',  ( -3.219174618344376363E-15, 37.50000000000000000, -52.57311121191334990 ) ) ;
#13273 = CARTESIAN_POINT ( 'NONE',  ( 15.40903463028481113, 49.32187500034139305, -47.42413220539094709 ) ) ;
#13274 = CARTESIAN_POINT ( 'NONE',  ( -37.77664397204045343, 25.00000000000000355, 13.15010152849403369 ) ) ;
#13275 = VERTEX_POINT ( 'NONE', #6850 ) ;
#13276 = CARTESIAN_POINT ( 'NONE',  ( 30.81806926056962936, 41.22187500034139873, -42.41743335407647209 ) ) ;
#13277 = ORIENTED_EDGE ( 'NONE', *, *, #8173, .T. ) ;
#13278 = VERTEX_POINT ( 'NONE', #1827 ) ;
#13279 = PLANE ( 'NONE',  #5529 ) ;
#13280 = CARTESIAN_POINT ( 'NONE',  ( 5.510910596163089556E-15, 217.0000000000000284, -45.00000000000000000 ) ) ;
#13281 = LINE ( 'NONE', #8292, #6915 ) ;
#13282 = CARTESIAN_POINT ( 'NONE',  ( 30.90169943749475223, 36.48125000068279888, 42.53254041760199300 ) ) ;
#13283 = CARTESIAN_POINT ( 'NONE',  ( -3.210462471511496205E-15, 45.35937500034139447, -52.43083105670540789 ) ) ;
#13284 = CARTESIAN_POINT ( 'NONE',  ( 40.34137639590981905, 48.65937500034139873, 29.30972558990010768 ) ) ;
#13285 = LINE ( 'NONE', #10394, #6635 ) ;
#13286 = CARTESIAN_POINT ( 'NONE',  ( -2.547328955960238000E-13, 34.28125000068279604, 49.99999999999999289 ) ) ;
#13287 = SURFACE_SIDE_STYLE ('',( #16118 ) ) ;
#13288 = CARTESIAN_POINT ( 'NONE',  ( 0.000000000000000000, 102.0000000000000142, -5.000000000000000000 ) ) ;
#13289 = DIRECTION ( 'NONE',  ( 0.000000000000000000, -0.000000000000000000, 1.000000000000000000 ) ) ;
#13290 = DIRECTION ( 'NONE',  ( 0.000000000000000000, 0.000000000000000000, 1.000000000000000000 ) ) ;
#13291 = CARTESIAN_POINT ( 'NONE',  ( 30.90169943749473802, 37.29999999999999716, -42.53254041760200721 ) ) ;
#13292 = EDGE_LOOP ( 'NONE', ( #13503, #9177, #5682 ) ) ;
#13293 = EDGE_CURVE ( 'NONE', #7383, #4055, #9494, .T. ) ;
#13294 = CARTESIAN_POINT ( 'NONE',  ( -15.40903463028481646, 29.45937500034139589, -47.42413220539093999 ) ) ;
#13295 = ORIENTED_EDGE ( 'NONE', *, *, #3264, .T. ) ;
#13296 = VERTEX_POINT ( 'NONE', #5753 ) ;
#13297 = VERTEX_POINT ( 'NONE', #14379 ) ;
#13298 = CARTESIAN_POINT ( 'NONE',  ( 30.90169943749475578, 40.48125000068279888, 42.53254041760200010 ) ) ;
#13299 = DIRECTION ( 'NONE',  ( -0.2079116908177665590, 0.9781476007338041345, 0.000000000000000000 ) ) ;
#13300 = CARTESIAN_POINT ( 'NONE',  ( -40.34137639590981195, 24.05937500034139731, 29.30972558990012189 ) ) ;
#13301 = ORIENTED_EDGE ( 'NONE', *, *, #13600, .F. ) ;
#13302 = SURFACE_STYLE_FILL_AREA ( #5832 ) ;
#13303 = CARTESIAN_POINT ( 'NONE',  ( -40.45084971874737079, 48.20000000000000284, 29.38926261462367151 ) ) ;
#13304 = CARTESIAN_POINT ( 'NONE',  ( 30.90169943749473802, 23.29999999999999716, -42.53254041760200721 ) ) ;
#13305 = CARTESIAN_POINT ( 'NONE',  ( 0.000000000000000000, 0.000000000000000000, 0.000000000000000000 ) ) ;
#13306 = CARTESIAN_POINT ( 'NONE',  ( 40.34137639590981195, 31.12187500034139731, -29.30972558990011834 ) ) ;
#13307 = DIRECTION ( 'NONE',  ( -0.9510565162951503115, -0.3090169943749574988, 0.000000000000000000 ) ) ;
#13308 = ADVANCED_FACE ( 'NONE', ( #9574 ), #11811, .T. ) ;
#13309 = PRODUCT_RELATED_PRODUCT_CATEGORY ( 'part', '', ( #5220 ) ) ;
#13310 = CARTESIAN_POINT ( 'NONE',  ( -49.99999999999999289, 42.09999999999999432, 16.24598481164533226 ) ) ;
#13311 = CARTESIAN_POINT ( 'NONE',  ( -40.34137639590981195, 24.12187500034139731, 29.30972558990012189 ) ) ;
#13312 = LINE ( 'NONE', #16050, #6856 ) ;
#13313 = CARTESIAN_POINT ( 'NONE',  ( 40.45084971874737789, 32.80000000000000426, 29.38926261462365375 ) ) ;
#13314 = CARTESIAN_POINT ( 'NONE',  ( -49.86468353124999453, 23.75937500034140015, -16.20201782572375393 ) ) ;
#13315 = LINE ( 'NONE', #3340, #15479 ) ;
#13316 = EDGE_CURVE ( 'NONE', #6916, #306, #13141, .T. ) ;
#13317 = ORIENTED_EDGE ( 'NONE', *, *, #2263, .F. ) ;
#13318 = CARTESIAN_POINT ( 'NONE',  ( -49.86468353124999453, 29.75937500034139305, -16.20201782572375393 ) ) ;
#13319 = ORIENTED_EDGE ( 'NONE', *, *, #3110, .F. ) ;
#13320 = PLANE ( 'NONE',  #6288 ) ;
#13321 = CARTESIAN_POINT ( 'NONE',  ( -49.86468353124999453, 43.75937500034140015, -16.20201782572375393 ) ) ;
#13322 = EDGE_CURVE ( 'NONE', #9791, #14391, #572, .T. ) ;
#13323 = CARTESIAN_POINT ( 'NONE',  ( 25.56848793686308596, 282.5058351977237407, 10.28424396843140620 ) ) ;
#13324 = CARTESIAN_POINT ( 'NONE',  ( -5.823736356558307894E-14, 44.28125000068280315, 50.00000000000000000 ) ) ;
#13325 = CARTESIAN_POINT ( 'NONE',  ( -15.40903463028480580, 28.32187500034139660, 47.42413220539094709 ) ) ;
#13326 = CARTESIAN_POINT ( 'NONE',  ( -40.34137639590981195, 34.05937500034139731, 29.30972558990012189 ) ) ;
#13327 = LINE ( 'NONE', #1851, #11057 ) ;
#13328 = CARTESIAN_POINT ( 'NONE',  ( 15.40903463028482356, 30.52187500034139589, 47.42413220539093999 ) ) ;
#13329 = CARTESIAN_POINT ( 'NONE',  ( 49.99999999999999289, 41.10000000000000853, -16.24598481164532160 ) ) ;
#13330 = CARTESIAN_POINT ( 'NONE',  ( 40.34137639590981905, 44.65937500034139163, 29.30972558990010768 ) ) ;
#13331 = CARTESIAN_POINT ( 'NONE',  ( 40.34137639590981905, 44.72187500034139163, 29.30972558990010768 ) ) ;
#13332 = EDGE_CURVE ( 'NONE', #4817, #5627, #8300, .T. ) ;
#13333 = CARTESIAN_POINT ( 'NONE',  ( 9.657523855033129090E-15, 48.50000000000000000, 52.57311121191334990 ) ) ;
#13334 = ORIENTED_EDGE ( 'NONE', *, *, #5685, .T. ) ;
#13335 = CARTESIAN_POINT ( 'NONE',  ( -49.99999999999999289, 27.88125000068280102, 16.24598481164533226 ) ) ;
#13336 = ORIENTED_EDGE ( 'NONE', *, *, #4334, .T. ) ;
#13337 = EDGE_LOOP ( 'NONE', ( #10749, #9304, #16101, #16453 ) ) ;
#13339 = EDGE_CURVE ( 'NONE', #3858, #4499, #5868, .T. ) ;
#13338 = CARTESIAN_POINT ( 'NONE',  ( -49.99999999999999289, 27.88125000068279746, 16.24598481164533226 ) ) ;
#13340 = VERTEX_POINT ( 'NONE', #5667 ) ;
#13341 = AXIS2_PLACEMENT_3D ( 'NONE', #11143, #11053, #12377 ) ;
#13342 = CARTESIAN_POINT ( 'NONE',  ( 3.987376076617427767, 6.145737624504234553, 101.6666710451724214 ) ) ;
#13343 = CARTESIAN_POINT ( 'NONE',  ( -15.40903463028481646, 39.52187500034139589, -47.42413220539093999 ) ) ;
#13344 = CARTESIAN_POINT ( 'NONE',  ( 49.86468353124999453, 20.95937500034138878, -16.20201782572376459 ) ) ;
#13345 = DIRECTION ( 'NONE',  ( 0.000000000000000000, 1.000000000000000000, 0.000000000000000000 ) ) ;
#13346 = PRODUCT_CONTEXT ( 'NONE', #15337, 'mechanical' ) ;
#13347 = CARTESIAN_POINT ( 'NONE',  ( -15.45084971874737256, 39.60000000000000142, -47.55282581475767500 ) ) ;
#13348 = EDGE_CURVE ( 'NONE', #3492, #1639, #2016, .T. ) ;
#13349 =( BOUNDED_CURVE ( )  B_SPLINE_CURVE ( 2, ( #11474, #6169, #3677, #8812, #13876, #8733, #11400, #3832, #9726, #12801, #15202, #3916, #8897 ),
 .UNSPECIFIED., .F., .T. ) 
 B_SPLINE_CURVE_WITH_KNOTS ( ( 3, 2, 2, 2, 2, 2, 3 ),
 ( 0.1499999999999999944, 0.1533333333333333215, 0.1600000000000000033, 0.1666666666666666574, 0.1733333333333333393, 0.1799999999999999933, 0.1833333333333333481 ),
 .UNSPECIFIED. ) 
 CURVE ( )  GEOMETRIC_REPRESENTATION_ITEM ( )  RATIONAL_B_SPLINE_CURVE ( ( 0.9755282581475768211, 0.9755282581475768211, 1.000000000000000000, 0.9510565162951535312, 1.000000000000000000, 0.9510565162951535312, 1.000000000000000000, 0.9510565162951535312, 1.000000000000000000, 0.9510565162951535312, 1.000000000000000000, 0.9755282581475765991, 0.9755282581475767101 ) ) 
 REPRESENTATION_ITEM ( '' )  );
#13350 = CARTESIAN_POINT ( 'NONE',  ( 30.81806926056962936, 39.22187500034139873, -42.41743335407647209 ) ) ;
#13351 = CARTESIAN_POINT ( 'NONE',  ( 7.919222016226693306, 30.55125428154684286, 50.00000000000003553 ) ) ;
#13352 = ORIENTED_EDGE ( 'NONE', *, *, #6451, .F. ) ;
#13353 = AXIS2_PLACEMENT_3D ( 'NONE', #16064, #9669, #7353 ) ;
#13354 = CARTESIAN_POINT ( 'NONE',  ( -15.40903463028480580, 42.32187500034139305, 47.42413220539094709 ) ) ;
#13355 = ORIENTED_EDGE ( 'NONE', *, *, #11930, .T. ) ;
#13356 = ORIENTED_EDGE ( 'NONE', *, *, #16286, .T. ) ;
#13357 = VERTEX_POINT ( 'NONE', #15711 ) ;
#13358 = CARTESIAN_POINT ( 'NONE',  ( -15.45084971874737256, 39.38125000068279746, -47.55282581475767500 ) ) ;
#13359 = CARTESIAN_POINT ( 'NONE',  ( 0.000000000000000000, 279.6527036446661327, 0.000000000000000000 ) ) ;
#13360 = CARTESIAN_POINT ( 'NONE',  ( -6.251299836021416922, 37.76994598419257443, 102.0000000000000142 ) ) ;
#13361 = CARTESIAN_POINT ( 'NONE',  ( 15.40544456622774661, 14.18301270189236973, 101.0000000000000000 ) ) ;
#13362 = CARTESIAN_POINT ( 'NONE',  ( 9.631387414534489405E-15, 38.35937500034139447, 52.43083105670540789 ) ) ;
#13363 = PLANE ( 'NONE',  #15208 ) ;
#13364 = CARTESIAN_POINT ( 'NONE',  ( 50.00000000000000000, 25.00000000000000000, -6.123233995736766085E-15 ) ) ;
#13365 = DIRECTION ( 'NONE',  ( 0.000000000000000000, -0.000000000000000000, 1.000000000000000000 ) ) ;
#13366 =( NAMED_UNIT ( * ) SI_UNIT ( $, .STERADIAN. ) SOLID_ANGLE_UNIT ( ) );
#13367 = CARTESIAN_POINT ( 'NONE',  ( 2.939893647802748866, 6.264020653511243708, 102.0000000000000142 ) ) ;
#13368 = DIRECTION ( 'NONE',  ( 0.000000000000000000, 1.000000000000000000, 0.000000000000000000 ) ) ;
#13369 = CARTESIAN_POINT ( 'NONE',  ( 50.00000000000000000, 41.00000000000000000, -6.123233995736766085E-15 ) ) ;
#13370 = DIRECTION ( 'NONE',  ( 1.000000000000000000, 0.000000000000000000, 0.000000000000000000 ) ) ;
#13371 = ORIENTED_EDGE ( 'NONE', *, *, #10222, .T. ) ;
#13372 = CARTESIAN_POINT ( 'NONE',  ( -49.86468353125000164, 31.85937500034139447, 0.000000000000000000 ) ) ;
#13373 = ORIENTED_EDGE ( 'NONE', *, *, #14892, .F. ) ;
#13374 = ORIENTED_EDGE ( 'NONE', *, *, #11747, .F. ) ;
#13375 = ORIENTED_EDGE ( 'NONE', *, *, #8730, .F. ) ;
#13376 = CARTESIAN_POINT ( 'NONE',  ( 40.45084971874737079, 44.98125000068279888, -29.38926261462366440 ) ) ;
#13377 = DIRECTION ( 'NONE',  ( -0.000000000000000000, 1.000000000000000000, -0.000000000000000000 ) ) ;
#13378 = DIRECTION ( 'NONE',  ( 0.000000000000000000, 0.000000000000000000, -1.000000000000000000 ) ) ;
#13379 = ORIENTED_EDGE ( 'NONE', *, *, #11795, .T. ) ;
#13380 = CARTESIAN_POINT ( 'NONE',  ( 0.000000000000000000, 247.0000000000000284, 0.000000000000000000 ) ) ;
#13381 = CARTESIAN_POINT ( 'NONE',  ( 40.45084971874737789, 34.80000000000000426, 29.38926261462365375 ) ) ;
#13382 = DIRECTION ( 'NONE',  ( 0.000000000000000000, 1.000000000000000000, 0.000000000000000000 ) ) ;
#13383 = LINE ( 'NONE', #11159, #1018 ) ;
#13384 = CARTESIAN_POINT ( 'NONE',  ( -7.919222016226934890, 32.44874571845316069, 49.99999999999996447 ) ) ;
#13385 = CARTESIAN_POINT ( 'NONE',  ( 40.45084971874737079, 36.98125000068279888, -29.38926261462366440 ) ) ;
#13386 = CARTESIAN_POINT ( 'NONE',  ( -45.11452830843730766, 20.00000000000000711, 21.24066852005664430 ) ) ;
#13387 = CARTESIAN_POINT ( 'NONE',  ( 9.631387414534489405E-15, 24.42187500034139447, 52.43083105670540789 ) ) ;
#13388 = DIRECTION ( 'NONE',  ( 1.000000000000000000, 2.141144404634230516E-14, 0.000000000000000000 ) ) ;
#13389 = CARTESIAN_POINT ( 'NONE',  ( 40.45084971874737789, 30.80000000000000071, 29.38926261462365375 ) ) ;
#13390 = CARTESIAN_POINT ( 'NONE',  ( 30.81806926056962936, 23.15937500034139873, -42.41743335407647209 ) ) ;
#13391 = CARTESIAN_POINT ( 'NONE',  ( 15.40903463028481113, 47.25937500034140015, -47.42413220539094709 ) ) ;
#13392 = ORIENTED_EDGE ( 'NONE', *, *, #1880, .F. ) ;
#13393 = SHAPE_REPRESENTATION ( 'Speed Control Knob & Dial', ( #15812 ), #16077 ) ;
#13394 = DIRECTION ( 'NONE',  ( 0.1984322509960772252, -0.9259215214979057418, -0.3213938048432687378 ) ) ;
#13395 = EDGE_LOOP ( 'NONE', ( #11824, #15234, #6054, #16261 ) ) ;
#13396 = CARTESIAN_POINT ( 'NONE',  ( -2.020067798342124465, 103.3979712344554116, 5.000000000000000000 ) ) ;
#13397 = CARTESIAN_POINT ( 'NONE',  ( 15.40903463028482356, 38.45937500034139589, 47.42413220539093999 ) ) ;
#13398 = CARTESIAN_POINT ( 'NONE',  ( 1.508581220285784909E-14, 52.00000000000002132, 44.99999999999998579 ) ) ;
#13399 = CARTESIAN_POINT ( 'NONE',  ( 40.45084971874737079, 35.20000000000000284, -29.38926261462366440 ) ) ;
#13400 = CARTESIAN_POINT ( 'NONE',  ( 7.919222016226809657, 45.22999571913594963, -50.00000000000000000 ) ) ;
#13401 = CARTESIAN_POINT ( 'NONE',  ( 30.81806926056964002, 32.62187500034140442, 42.41743335407647209 ) ) ;
#13402 = CARTESIAN_POINT ( 'NONE',  ( -49.86468353125000164, 29.85937500034139802, 0.000000000000000000 ) ) ;
#13403 = CARTESIAN_POINT ( 'NONE',  ( 9.631387414534489405E-15, 30.42187500034139447, 52.43083105670540789 ) ) ;
#13404 = CARTESIAN_POINT ( 'NONE',  ( -8.660254037844387298, 28.00000000000000355, 5.000000000000000000 ) ) ;
#13405 = CARTESIAN_POINT ( 'NONE',  ( -30.81806926056962226, 44.15937500034139163, 42.41743335407647919 ) ) ;
#13406 = CARTESIAN_POINT ( 'NONE',  ( -30.81806926056963292, 35.62187500034140442, -42.41743335407647209 ) ) ;
#13407 = VECTOR ( 'NONE', #13786, 1000.000000000000000 ) ;
#13408 = ADVANCED_FACE ( 'NONE', ( #4508 ), #15552, .T. ) ;
#13409 = CARTESIAN_POINT ( 'NONE',  ( 49.86468353125001585, 22.82187500034138949, 16.20201782572375038 ) ) ;
#13410 =( GEOMETRIC_REPRESENTATION_CONTEXT ( 3 ) GLOBAL_UNCERTAINTY_ASSIGNED_CONTEXT ( ( #1435 ) ) GLOBAL_UNIT_ASSIGNED_CONTEXT ( ( #1651, #4247, #15622 ) ) REPRESENTATION_CONTEXT ( 'NONE', 'WORKASPACE' ) );
#13411 = VERTEX_POINT ( 'NONE', #4424 ) ;
#13412 = ADVANCED_FACE ( 'NONE', ( #8237 ), #14618, .F. ) ;
#13413 = CARTESIAN_POINT ( 'NONE',  ( 40.34137639590981905, 44.65937500034139163, 29.30972558990010768 ) ) ;
#13414 = ORIENTED_EDGE ( 'NONE', *, *, #5294, .F. ) ;
#13416 = EDGE_CURVE ( 'NONE', #3156, #14668, #3001, .T. ) ;
#13415 = CARTESIAN_POINT ( 'NONE',  ( 50.00000000000000711, 30.68125000068279462, 16.24598481164530739 ) ) ;
#13417 = EDGE_LOOP ( 'NONE', ( #1292, #6317, #7644, #9972 ) ) ;
#13418 = VECTOR ( 'NONE', #13769, 1000.000000000000114 ) ;
#13419 = AXIS2_PLACEMENT_3D ( 'NONE', #10636, #1723, #10708 ) ;
#13420 = VECTOR ( 'NONE', #5470, 1000.000000000000000 ) ;
#13421 = AXIS2_PLACEMENT_3D ( 'NONE', #13027, #1795, #5712 ) ;
#13422 = EDGE_CURVE ( 'NONE', #8515, #11147, #3625, .T. ) ;
#13423 = FACE_OUTER_BOUND ( 'NONE', #694, .T. ) ;
#13424 = CARTESIAN_POINT ( 'NONE',  ( 49.86468353125000164, 38.92187500034139447, -6.106662507704105588E-15 ) ) ;
#13425 = CARTESIAN_POINT ( 'NONE',  ( -49.86468353125000164, 49.92187500034140157, 0.000000000000000000 ) ) ;
#13426 = STYLED_ITEM ( 'NONE', ( #8963 ), #1465 ) ;
#13427 = DIRECTION ( 'NONE',  ( -0.9961946980917455452, -0.08715574274765824914, 0.000000000000000000 ) ) ;
#13428 = CARTESIAN_POINT ( 'NONE',  ( -40.34137639590981195, 24.12187500034139731, 29.30972558990012189 ) ) ;
#13429 = CIRCLE ( 'NONE', #11103, 79.49773270518484480 ) ;
#13430 = APPLICATION_PROTOCOL_DEFINITION ( 'draft international standard', 'automotive_design', 1998, #6668 ) ;
#13431 = CARTESIAN_POINT ( 'NONE',  ( -40.45084971874737789, 37.79999999999999716, -29.38926261462365730 ) ) ;
#13432 = CARTESIAN_POINT ( 'NONE',  ( 9.631387414534489405E-15, 38.42187500034139447, 52.43083105670540789 ) ) ;
#13433 = CARTESIAN_POINT ( 'NONE',  ( 7.500000000000000000, 40.00000000000000711, 39.29058411375427795 ) ) ;
#13434 = AXIS2_PLACEMENT_3D ( 'NONE', #9825, #3505, #4674 ) ;
#13435 = ORIENTED_EDGE ( 'NONE', *, *, #10194, .T. ) ;
#13436 = AXIS2_PLACEMENT_3D ( 'NONE', #1770, #9422, #3103 ) ;
#13437 = CARTESIAN_POINT ( 'NONE',  ( 40.34137639590981195, 39.12187500034139731, -29.30972558990011834 ) ) ;
#13438 = ORIENTED_EDGE ( 'NONE', *, *, #13416, .T. ) ;
#13439 = ORIENTED_EDGE ( 'NONE', *, *, #14107, .F. ) ;
#13440 = VERTEX_POINT ( 'NONE', #2924 ) ;
#13441 = EDGE_CURVE ( 'NONE', #3153, #3704, #13065, .T. ) ;
#13442 = DIRECTION ( 'NONE',  ( 1.067350013832299517E-17, 0.9961946980917455452, -0.08715574274765836016 ) ) ;
#13443 = CARTESIAN_POINT ( 'NONE',  ( 0.000000000000000000, 193.4213562373095385, 0.000000000000000000 ) ) ;
#13444 = CARTESIAN_POINT ( 'NONE',  ( -30.90169943749473447, 22.08125000068279320, 42.53254041760200721 ) ) ;
#13445 = CYLINDRICAL_SURFACE ( 'NONE', #10595, 50.00000000000000000 ) ;
#13446 = CARTESIAN_POINT ( 'NONE',  ( 15.40903463028482356, 38.45937500034139589, 47.42413220539093999 ) ) ;
#13447 = STYLED_ITEM ( 'NONE', ( #161 ), #14144 ) ;
#13448 = CARTESIAN_POINT ( 'NONE',  ( 49.86468353124999453, 46.95937500034139589, -16.20201782572376104 ) ) ;
#13449 = ADVANCED_FACE ( 'NONE', ( #5519 ), #15638, .F. ) ;
#13450 = CARTESIAN_POINT ( 'NONE',  ( -40.45084971874737789, 29.80000000000000071, -29.38926261462365730 ) ) ;
#13451 = AXIS2_PLACEMENT_3D ( 'NONE', #5663, #493, #6846 ) ;
#13452 = FACE_OUTER_BOUND ( 'NONE', #11249, .T. ) ;
#13453 = CARTESIAN_POINT ( 'NONE',  ( 0.5000000000000000000, 244.0000000000000284, -49.99999999999999289 ) ) ;
#13454 = CARTESIAN_POINT ( 'NONE',  ( -49.99999999999999289, 35.88125000068279746, 16.24598481164533226 ) ) ;
#13455 = CARTESIAN_POINT ( 'NONE',  ( 6.725310538855729270, 29.22831317314791733, 101.0000000000000000 ) ) ;
#13456 = CARTESIAN_POINT ( 'NONE',  ( 20.00000000000000000, 312.0000000000000568, 4.625929269271485322E-15 ) ) ;
#13457 = ORIENTED_EDGE ( 'NONE', *, *, #7051, .T. ) ;
#13458 = CARTESIAN_POINT ( 'NONE',  ( -40.34137639590981905, 29.65937500034139518, -29.30972558990011478 ) ) ;
#13459 = VECTOR ( 'NONE', #5843, 1000.000000000000000 ) ;
#13460 = VERTEX_POINT ( 'NONE', #13468 ) ;
#13461 = ORIENTED_EDGE ( 'NONE', *, *, #9870, .F. ) ;
#13462 = EDGE_LOOP ( 'NONE', ( #4025, #4506, #1438, #14692 ) ) ;
#13463 = CARTESIAN_POINT ( 'NONE',  ( -49.99999999999999289, 45.68125000068280173, -16.24598481164531449 ) ) ;
#13464 = CARTESIAN_POINT ( 'NONE',  ( -2.445080149700054274E-14, 46.50000000000000711, 50.00000000000000000 ) ) ;
#13465 = CARTESIAN_POINT ( 'NONE',  ( 15.45084971874737789, 28.60000000000000142, 47.55282581475767500 ) ) ;
#13466 = ORIENTED_EDGE ( 'NONE', *, *, #7735, .T. ) ;
#13467 = DIRECTION ( 'NONE',  ( 0.000000000000000000, 0.000000000000000000, -1.000000000000000000 ) ) ;
#13468 = CARTESIAN_POINT ( 'NONE',  ( 19.99999999999999289, 287.0000000000000568, -7.500000000000000000 ) ) ;
#13469 = CARTESIAN_POINT ( 'NONE',  ( -5.988468393965924008, 15.10823117958422301, 101.0000000000000000 ) ) ;
#13470 = DIRECTION ( 'NONE',  ( -0.000000000000000000, -1.000000000000000000, -0.000000000000000000 ) ) ;
#13471 = CARTESIAN_POINT ( 'NONE',  ( 30.27664397204074476, 25.00000000000000355, 26.14048258526015189 ) ) ;
#13472 = ADVANCED_FACE ( 'NONE', ( #3580 ), #16041, .F. ) ;
#13473 = CARTESIAN_POINT ( 'NONE',  ( -30.90169943749474513, 31.70000000000000639, -42.53254041760200721 ) ) ;
#13474 = EDGE_CURVE ( 'NONE', #1819, #11153, #3880, .T. ) ;
#13475 = CARTESIAN_POINT ( 'NONE',  ( -45.54143403682493840, 20.00000000000001066, 20.30922080093765203 ) ) ;
#13476 = CARTESIAN_POINT ( 'NONE',  ( -30.81806926056963292, 25.62187500034139731, -42.41743335407646498 ) ) ;
#13477 = FACE_OUTER_BOUND ( 'NONE', #1161, .T. ) ;
#13478 = CARTESIAN_POINT ( 'NONE',  ( 15.45084971874736723, 25.40000000000000213, -47.55282581475768211 ) ) ;
#13479 = CARTESIAN_POINT ( 'NONE',  ( -15.40903463028480580, 24.25937500034139660, 47.42413220539094709 ) ) ;
#13480 = CARTESIAN_POINT ( 'NONE',  ( 9.631387414534489405E-15, 48.35937500034140157, 52.43083105670540789 ) ) ;
#13481 = VERTEX_POINT ( 'NONE', #13710 ) ;
#13482 = CARTESIAN_POINT ( 'NONE',  ( 15.40903463028482356, 26.45937500034139589, 47.42413220539093999 ) ) ;
#13483 = ORIENTED_EDGE ( 'NONE', *, *, #4203, .T. ) ;
#13484 = CARTESIAN_POINT ( 'NONE',  ( -3.111920190527341144E-15, 45.50000000000000000, -50.00000000000000000 ) ) ;
#13485 = CARTESIAN_POINT ( 'NONE',  ( 40.34137639590981195, 33.05937500034139731, -29.30972558990011834 ) ) ;
#13486 = CARTESIAN_POINT ( 'NONE',  ( 40.45084971874737789, 40.58125000068280031, 29.38926261462365375 ) ) ;
#13487 = CARTESIAN_POINT ( 'NONE',  ( 50.00000000000000711, 28.68125000068279462, 16.24598481164530739 ) ) ;
#13488 = CARTESIAN_POINT ( 'NONE',  ( 24.78626291527386272, 25.00000000000000355, -5.650101528494135827 ) ) ;
#13489 = CARTESIAN_POINT ( 'NONE',  ( 15.40903463028481113, 29.32187500034139660, -47.42413220539094709 ) ) ;
#13490 = CARTESIAN_POINT ( 'NONE',  ( -30.81806926056963292, 31.55937500034139376, -42.41743335407646498 ) ) ;
#13491 = DIRECTION ( 'NONE',  ( 1.000000000000000000, 0.000000000000000000, 0.000000000000000000 ) ) ;
#13492 = CARTESIAN_POINT ( 'NONE',  ( 30.81806926056964002, 28.62187500034140086, 42.41743335407647209 ) ) ;
#13493 = DIRECTION ( 'NONE',  ( 0.000000000000000000, 0.000000000000000000, 1.000000000000000000 ) ) ;
#13494 = CARTESIAN_POINT ( 'NONE',  ( -15.40903463028481646, 47.45937500034139589, -47.42413220539093999 ) ) ;
#13495 = CARTESIAN_POINT ( 'NONE',  ( -15.40903463028481646, 39.52187500034139589, -47.42413220539093999 ) ) ;
#13496 = SHAPE_REPRESENTATION ( 'Heavy Glass Blender Jar Body', ( #15812 ), #11844 ) ;
#13497 = CARTESIAN_POINT ( 'NONE',  ( -49.86468353124999453, 23.82187500034139305, -16.20201782572375393 ) ) ;
#13498 = ORIENTED_EDGE ( 'NONE', *, *, #2914, .T. ) ;
#13499 = CARTESIAN_POINT ( 'NONE',  ( 49.86468353125001585, 44.75937500034139305, 16.20201782572375038 ) ) ;
#13500 = EDGE_LOOP ( 'NONE', ( #11383, #1642, #2219, #10969 ) ) ;
#13501 = CARTESIAN_POINT ( 'NONE',  ( 9.657523855033129090E-15, 24.28125000068279959, 52.57311121191334990 ) ) ;
#13502 = AXIS2_PLACEMENT_3D ( 'NONE', #13047, #10715, #5649 ) ;
#13503 = ORIENTED_EDGE ( 'NONE', *, *, #16408, .F. ) ;
#13504 = CARTESIAN_POINT ( 'NONE',  ( 40.45084971874737079, 40.98125000068279888, -29.38926261462366440 ) ) ;
#13505 = CARTESIAN_POINT ( 'NONE',  ( 15.40903463028482356, 40.52187500034139589, 47.42413220539093999 ) ) ;
#13506 = CARTESIAN_POINT ( 'NONE',  ( 40.34137639590981905, 46.72187500034139873, 29.30972558990010768 ) ) ;
#13507 = CARTESIAN_POINT ( 'NONE',  ( 2.600676159226420495E-13, 31.49999999999999289, -49.99999999999999289 ) ) ;
#13508 = CARTESIAN_POINT ( 'NONE',  ( -30.81806926056963292, 23.62187500034139731, -42.41743335407647209 ) ) ;
#13509 = ITEM_DEFINED_TRANSFORMATION ( 'NONE', 'NONE', #1752,  #15812 ) ;
#13510 = CARTESIAN_POINT ( 'NONE',  ( -30.90169943749473802, 34.08125000068279320, 42.53254041760200721 ) ) ;
#13511 = EDGE_CURVE ( 'NONE', #12729, #12156, #12302, .T. ) ;
#13512 = VECTOR ( 'NONE', #1573, 1000.000000000000000 ) ;
#13513 = CARTESIAN_POINT ( 'NONE',  ( 15.40903463028481113, 41.32187500034140015, -47.42413220539094709 ) ) ;
#13514 = CARTESIAN_POINT ( 'NONE',  ( -27.49424662897630256, 282.6608420050619088, -7.488493257954155879 ) ) ;
#13515 = VERTEX_POINT ( 'NONE', #16291 ) ;
#13516 = CARTESIAN_POINT ( 'NONE',  ( -40.34137639590981195, 42.12187500034139731, 29.30972558990012189 ) ) ;
#13517 = CARTESIAN_POINT ( 'NONE',  ( -40.45084971874737079, 43.98125000068279888, 29.38926261462367151 ) ) ;
#13518 = EDGE_CURVE ( 'NONE', #9791, #13440, #13565, .T. ) ;
#13519 = VERTEX_POINT ( 'NONE', #12144 ) ;
#13520 = B_SPLINE_CURVE_WITH_KNOTS ( 'NONE', 3,
 ( #12228, #12399, #9903, #3330 ),
 .UNSPECIFIED., .F., .F.,
 ( 4, 4 ),
 ( 0.000000000000000000, 0.01241723871866257621 ),
 .UNSPECIFIED. ) ;
#13521 = EDGE_LOOP ( 'NONE', ( #1955, #489, #12543, #15574 ) ) ;
#13522 = ORIENTED_EDGE ( 'NONE', *, *, #800, .F. ) ;
#13523 = CARTESIAN_POINT ( 'NONE',  ( -40.45084971874737789, 39.58125000068280031, -29.38926261462365730 ) ) ;
#13524 = CARTESIAN_POINT ( 'NONE',  ( 15.53071739328000334, 28.07196708982297295, 102.0000000000000142 ) ) ;
#13525 = ADVANCED_FACE ( 'NONE', ( #6160 ), #9742, .F. ) ;
#13526 = CARTESIAN_POINT ( 'NONE',  ( 7.919222016226809657, 27.44874571845315003, -50.00000000000000000 ) ) ;
#13527 = DIRECTION ( 'NONE',  ( 0.000000000000000000, 0.000000000000000000, 1.000000000000000000 ) ) ;
#13528 = CIRCLE ( 'NONE', #3716, 17.50000000000000000 ) ;
#13529 = CARTESIAN_POINT ( 'NONE',  ( 40.34137639590981905, 38.65937500034139873, 29.30972558990010768 ) ) ;
#13530 = CARTESIAN_POINT ( 'NONE',  ( 9.574901606694759531E-15, 52.00000000000001421, -2.191293403013901479E-14 ) ) ;
#13531 = CARTESIAN_POINT ( 'NONE',  ( 49.99999999999999289, 25.10000000000000142, -16.24598481164532160 ) ) ;
#13532 = CARTESIAN_POINT ( 'NONE',  ( 1.293669679204937499E-13, 37.50000000000000711, -50.00000000000000000 ) ) ;
#13533 = FILL_AREA_STYLE_COLOUR ( '', #11037 ) ;
#13534 = FACE_OUTER_BOUND ( 'NONE', #15613, .T. ) ;
#13535 = CARTESIAN_POINT ( 'NONE',  ( -3.111920190527341144E-15, 45.50000000000000000, -50.00000000000000000 ) ) ;
#13536 = DIRECTION ( 'NONE',  ( 0.9781476007338042455, 0.2079116908177664758, 0.000000000000000000 ) ) ;
#13537 = ORIENTED_EDGE ( 'NONE', *, *, #10486, .T. ) ;
#13538 = CARTESIAN_POINT ( 'NONE',  ( -15.40903463028480580, 34.25937500034139305, 47.42413220539094709 ) ) ;
#13539 = ORIENTED_EDGE ( 'NONE', *, *, #2520, .T. ) ;
#13540 = ORIENTED_EDGE ( 'NONE', *, *, #6349, .F. ) ;
#13541 = VERTEX_POINT ( 'NONE', #16136 ) ;
#13542 = CARTESIAN_POINT ( 'NONE',  ( -15.45084971874737256, 41.38125000068279746, -47.55282581475767500 ) ) ;
#13543 = CARTESIAN_POINT ( 'NONE',  ( 2.978552182361884590E-14, 47.50000000000000711, -50.00000000000000000 ) ) ;
#13544 = FACE_OUTER_BOUND ( 'NONE', #8455, .T. ) ;
#13545 = EDGE_CURVE ( 'NONE', #10216, #13275, #434, .T. ) ;
#13546 = ORIENTED_EDGE ( 'NONE', *, *, #12231, .T. ) ;
#13547 = CARTESIAN_POINT ( 'NONE',  ( -49.99999999999999289, 47.68125000068280173, -16.24598481164531449 ) ) ;
#13548 = CARTESIAN_POINT ( 'NONE',  ( 0.000000000000000000, 22.50000000000000000, 101.0000000000000000 ) ) ;
#13549 = FACE_OUTER_BOUND ( 'NONE', #5886, .T. ) ;
#13550 = FACE_OUTER_BOUND ( 'NONE', #2498, .T. ) ;
#13551 = CARTESIAN_POINT ( 'NONE',  ( 13.33429048796497085, 33.83343271840296751, 101.0000000000000000 ) ) ;
#13552 = CARTESIAN_POINT ( 'NONE',  ( 50.00000000000000711, 38.89999999999999858, 16.24598481164530739 ) ) ;
#13553 = CARTESIAN_POINT ( 'NONE',  ( 1.293669679204937499E-13, 41.50000000000000000, -50.00000000000000000 ) ) ;
#13554 = CARTESIAN_POINT ( 'NONE',  ( -40.45084971874737079, 45.98125000068279888, 29.38926261462367151 ) ) ;
#13555 = DIRECTION ( 'NONE',  ( 0.000000000000000000, -5.551115123125782702E-17, 1.000000000000000000 ) ) ;
#13556 = CARTESIAN_POINT ( 'NONE',  ( -30.90169943749473802, 30.29999999999999716, 42.53254041760200721 ) ) ;
#13557 = CARTESIAN_POINT ( 'NONE',  ( -15.40903463028480580, 28.25937500034139660, 47.42413220539094709 ) ) ;
#13558 = CARTESIAN_POINT ( 'NONE',  ( -49.99999999999999289, 29.89999999999999858, -16.24598481164531449 ) ) ;
#13559 = ORIENTED_EDGE ( 'NONE', *, *, #12093, .T. ) ;
#13560 = CARTESIAN_POINT ( 'NONE',  ( 30.90169943749473802, 45.29999999999999005, -42.53254041760200721 ) ) ;
#13561 = EDGE_CURVE ( 'NONE', #14169, #15028, #9647, .T. ) ;
#13562 = VERTEX_POINT ( 'NONE', #8399 ) ;
#13563 = LINE ( 'NONE', #3688, #5501 ) ;
#13564 = CARTESIAN_POINT ( 'NONE',  ( 49.86468353125000164, 36.85937500034139447, -6.106662507704105588E-15 ) ) ;
#13565 = B_SPLINE_CURVE_WITH_KNOTS ( 'NONE', 3,
 ( #7165, #7326, #14872, #3501, #7242, #903, #4582, #9900, #12397, #2324, #988, #1069, #2235, #5833, #9821, #8554, #4669, #12477, #13625, #2404, #12225, #6088, #5917, #4927, #5998, #10977, #7408, #4764 ),
 .UNSPECIFIED., .F., .F.,
 ( 4, 2, 2, 2, 2, 2, 2, 2, 2, 2, 2, 2, 2, 4 ),
 ( 0.09705106074666051963, 0.09878860373063949596, 0.1005261467146184723, 0.1040012326825764527, 0.1057387756665554429, 0.1074763186505344331, 0.1092138616345134233, 0.1109514046184924135, 0.1144264905864503939, 0.1161640335704293980, 0.1179015765544083882, 0.1213766625223663825, 0.1231142055063453866, 0.1248517484903243768 ),
 .UNSPECIFIED. ) ;
#13566 = LINE ( 'NONE', #14718, #10534 ) ;
#13567 = CARTESIAN_POINT ( 'NONE',  ( -15.45084971874737256, 49.38125000068280457, -47.55282581475767500 ) ) ;
#13568 = DIRECTION ( 'NONE',  ( 0.8660254037844398178, 0.000000000000000000, 0.4999999999999978351 ) ) ;
#13569 = DIRECTION ( 'NONE',  ( -0.000000000000000000, -1.000000000000000000, -0.000000000000000000 ) ) ;
#13570 = CARTESIAN_POINT ( 'NONE',  ( 30.81806926056962936, 29.22187500034139873, -42.41743335407647209 ) ) ;
#13571 = CARTESIAN_POINT ( 'NONE',  ( -40.34137639590981905, 29.65937500034139518, -29.30972558990011478 ) ) ;
#13572 = CARTESIAN_POINT ( 'NONE',  ( -49.99999999999999289, 36.10000000000000142, 16.24598481164533226 ) ) ;
#13573 = CARTESIAN_POINT ( 'NONE',  ( -49.86468353124999453, 29.82187500034139660, -16.20201782572375393 ) ) ;
#13574 = DIRECTION ( 'NONE',  ( 0.3420201433256697676, 0.6644630243886755494, -0.6644630243886733290 ) ) ;
#13575 = CARTESIAN_POINT ( 'NONE',  ( -40.34137639590981195, 46.05937500034139731, 29.30972558990012189 ) ) ;
#13576 = CARTESIAN_POINT ( 'NONE',  ( 15.40903463028482356, 36.52187500034139589, 47.42413220539093999 ) ) ;
#13577 = CARTESIAN_POINT ( 'NONE',  ( -30.81806926056962226, 24.22187500034139163, 42.41743335407647919 ) ) ;
#13578 = ORIENTED_EDGE ( 'NONE', *, *, #8336, .F. ) ;
#13579 = CARTESIAN_POINT ( 'NONE',  ( 49.86468353124999453, 44.95937500034139589, -16.20201782572376104 ) ) ;
#13580 = ORIENTED_EDGE ( 'NONE', *, *, #13811, .T. ) ;
#13581 = CARTESIAN_POINT ( 'NONE',  ( 49.99999999999999289, 22.88125000068280102, -16.24598481164532160 ) ) ;
#13582 = VERTEX_POINT ( 'NONE', #6406 ) ;
#13583 = CARTESIAN_POINT ( 'NONE',  ( 0.000000000000000000, 20.00000000000000355, 0.000000000000000000 ) ) ;
#13584 = CARTESIAN_POINT ( 'NONE',  ( 49.86468353125001585, 36.82187500034140015, 16.20201782572375038 ) ) ;
#13585 = CARTESIAN_POINT ( 'NONE',  ( -30.81806926056962226, 48.22187500034139163, 42.41743335407647919 ) ) ;
#13586 = CARTESIAN_POINT ( 'NONE',  ( 15.45084971874737789, 30.60000000000000142, 47.55282581475767500 ) ) ;
#13587 =( BOUNDED_CURVE ( )  B_SPLINE_CURVE ( 2, ( #13507, #16179, #4808, #11198, #10938, #12518, #11276, #2283, #13755, #7451, #13586, #3378, #1108 ),
 .UNSPECIFIED., .F., .F. ) 
 B_SPLINE_CURVE_WITH_KNOTS ( ( 3, 2, 2, 2, 2, 2, 3 ),
 ( 0.6166666666666666963, 0.6199999999999999956, 0.6266666666666667052, 0.6333333333333333037, 0.6400000000000000133, 0.6466666666666666119, 0.6500000000000000222 ),
 .UNSPECIFIED. ) 
 CURVE ( )  GEOMETRIC_REPRESENTATION_ITEM ( )  RATIONAL_B_SPLINE_CURVE ( ( 0.9755282581475768211, 0.9755282581475771542, 1.000000000000000000, 0.9510565162951535312, 1.000000000000000000, 0.9510565162951535312, 1.000000000000000000, 0.9510565162951535312, 1.000000000000000000, 0.9510565162951535312, 1.000000000000000000, 0.9755282581475763770, 0.9755282581475768211 ) ) 
 REPRESENTATION_ITEM ( '' )  );
#13588 = ADVANCED_FACE ( 'NONE', ( #12719 ), #148, .T. ) ;
#13589 = CARTESIAN_POINT ( 'NONE',  ( 9.631387414534489405E-15, 26.42187500034139447, 52.43083105670540789 ) ) ;
#13590 = EDGE_CURVE ( 'NONE', #2880, #7989, #11048, .T. ) ;
#13591 = CARTESIAN_POINT ( 'NONE',  ( -40.45084971874737079, 35.98125000068279888, 29.38926261462367151 ) ) ;
#13592 = CARTESIAN_POINT ( 'NONE',  ( 15.40903463028481113, 39.32187500034140015, -47.42413220539094709 ) ) ;
#13593 = VERTEX_POINT ( 'NONE', #15119 ) ;
#13594 = CARTESIAN_POINT ( 'NONE',  ( 49.86468353125000164, 38.92187500034139447, -6.106662507704105588E-15 ) ) ;
#13595 = CARTESIAN_POINT ( 'NONE',  ( -15.45084971874736368, 32.18125000068279462, 47.55282581475768211 ) ) ;
#13596 = ORIENTED_EDGE ( 'NONE', *, *, #1414, .T. ) ;
#13597 = ORIENTED_EDGE ( 'NONE', *, *, #9779, .T. ) ;
#13598 = AXIS2_PLACEMENT_3D ( 'NONE', #10572, #15627, #7900 ) ;
#13599 = ORIENTED_EDGE ( 'NONE', *, *, #2775, .T. ) ;
#13600 = EDGE_CURVE ( 'NONE', #13993, #2741, #15635, .T. ) ;
#13601 = DIRECTION ( 'NONE',  ( 1.000000000000000000, 0.000000000000000000, -1.156482317317871478E-16 ) ) ;
#13602 = DIRECTION ( 'NONE',  ( 6.938893903907231459E-18, -1.000000000000000000, -5.551115123125782702E-17 ) ) ;
#13603 = CARTESIAN_POINT ( 'NONE',  ( -2.547328955960238000E-13, 22.49999999999999645, 49.99999999999999289 ) ) ;
#13604 = DIRECTION ( 'NONE',  ( -0.3213938048432674610, 0.7471788047720969717, 0.5817472440052537941 ) ) ;
#13605 = CARTESIAN_POINT ( 'NONE',  ( -15.40903463028480580, 40.25937500034139305, 47.42413220539094709 ) ) ;
#13606 = CARTESIAN_POINT ( 'NONE',  ( -30.81806926056962226, 48.15937500034139873, 42.41743335407647209 ) ) ;
#13607 = DIRECTION ( 'NONE',  ( 0.000000000000000000, 1.000000000000000000, 0.000000000000000000 ) ) ;
#13608 = CARTESIAN_POINT ( 'NONE',  ( -49.86468353125000164, 49.92187500034140157, 0.000000000000000000 ) ) ;
#13609 = DIRECTION ( 'NONE',  ( 0.000000000000000000, 0.000000000000000000, -1.000000000000000000 ) ) ;
#13610 = AXIS2_PLACEMENT_3D ( 'NONE', #11987, #5066, #8250 ) ;
#13611 = CARTESIAN_POINT ( 'NONE',  ( -15.45084971874737256, 33.60000000000000142, -47.55282581475767500 ) ) ;
#13612 = CARTESIAN_POINT ( 'NONE',  ( -30.90169943749473447, 42.30000000000000426, 42.53254041760200721 ) ) ;
#13613 = VERTEX_POINT ( 'NONE', #10143 ) ;
#13614 = ADVANCED_FACE ( 'NONE', ( #1486 ), #8805, .T. ) ;
#13615 = CARTESIAN_POINT ( 'NONE',  ( -40.34137639590981905, 23.65937500034139518, -29.30972558990011478 ) ) ;
#13616 = ORIENTED_EDGE ( 'NONE', *, *, #6218, .F. ) ;
#13617 = VERTEX_POINT ( 'NONE', #11639 ) ;
#13618 = ORIENTED_EDGE ( 'NONE', *, *, #11432, .F. ) ;
#13619 = CARTESIAN_POINT ( 'NONE',  ( -3.219174618344376363E-15, 41.28125000068280315, -52.57311121191334990 ) ) ;
#13620 = DIRECTION ( 'NONE',  ( 0.000000000000000000, 0.000000000000000000, 1.000000000000000000 ) ) ;
#13621 = LINE ( 'NONE', #823, #12610 ) ;
#13622 = ORIENTED_EDGE ( 'NONE', *, *, #10419, .T. ) ;
#13623 = CARTESIAN_POINT ( 'NONE',  ( -30.90169943749474513, 47.48125000068279888, -42.53254041760200721 ) ) ;
#13624 = DIRECTION ( 'NONE',  ( 0.000000000000000000, 0.000000000000000000, -1.000000000000000000 ) ) ;
#13625 = CARTESIAN_POINT ( 'NONE',  ( -8.844878598238441469, 7.388641928553207450, 98.30140974211549576 ) ) ;
#13626 = CARTESIAN_POINT ( 'NONE',  ( -7.580410092413954359, 102.0000000000000142, 5.000000000000000000 ) ) ;
#13627 = FACE_OUTER_BOUND ( 'NONE', #13217, .T. ) ;
#13628 = DIRECTION ( 'NONE',  ( -0.9510565162951503115, -0.3090169943749574988, 0.000000000000000000 ) ) ;
#13629 = FACE_OUTER_BOUND ( 'NONE', #1057, .T. ) ;
#13630 = EDGE_CURVE ( 'NONE', #8086, #4820, #6855, .T. ) ;
#13631 = CARTESIAN_POINT ( 'NONE',  ( -40.45084971874737789, 41.80000000000000426, -29.38926261462365730 ) ) ;
#13632 = CARTESIAN_POINT ( 'NONE',  ( -40.45084971874737079, 43.98125000068279888, 29.38926261462367151 ) ) ;
#13633 = DIRECTION ( 'NONE',  ( -0.000000000000000000, -1.000000000000000000, -0.000000000000000000 ) ) ;
#13634 = CARTESIAN_POINT ( 'NONE',  ( -30.90169943749473802, 28.30000000000000071, 42.53254041760200721 ) ) ;
#13635 = CARTESIAN_POINT ( 'NONE',  ( 49.86468353125001585, 20.75937500034140015, 16.20201782572375038 ) ) ;
#13636 = CARTESIAN_POINT ( 'NONE',  ( -7.919222016226752814, 41.33250428222964246, -50.00000000000000711 ) ) ;
#13637 = AXIS2_PLACEMENT_3D ( 'NONE', #2909, #7812, #9392 ) ;
#13638 = CARTESIAN_POINT ( 'NONE',  ( 15.40903463028482356, 48.45937500034140299, 47.42413220539093999 ) ) ;
#13639 = ORIENTED_EDGE ( 'NONE', *, *, #5945, .F. ) ;
#13640 = CARTESIAN_POINT ( 'NONE',  ( 49.99999999999999289, 45.10000000000000142, -16.24598481164532160 ) ) ;
#13641 = VERTEX_POINT ( 'NONE', #8890 ) ;
#13642 = CARTESIAN_POINT ( 'NONE',  ( 8.446640517145639571E-15, 48.49999999999999289, 50.00000000000000000 ) ) ;
#13643 = CARTESIAN_POINT ( 'NONE',  ( -49.86468353124999453, 35.75937500034140015, -16.20201782572375393 ) ) ;
#13644 = CARTESIAN_POINT ( 'NONE',  ( 14.03285685708579145, 13.82077604687259154, 102.0000000000000142 ) ) ;
#13645 = CARTESIAN_POINT ( 'NONE',  ( -6.668400408272873429E-15, 49.28125000068279604, -50.00000000000000000 ) ) ;
#13646 = ADVANCED_FACE ( 'NONE', ( #8978 ), #961, .F. ) ;
#13647 = CARTESIAN_POINT ( 'NONE',  ( 7.919222016226809657, 29.22999571913594963, -50.00000000000000000 ) ) ;
#13648 = VECTOR ( 'NONE', #3947, 1000.000000000000000 ) ;
#13649 = CARTESIAN_POINT ( 'NONE',  ( 0.000000000000000000, 193.4213562373095385, 0.000000000000000000 ) ) ;
#13650 = EDGE_CURVE ( 'NONE', #81, #15703, #4979, .T. ) ;
#13651 = CARTESIAN_POINT ( 'NONE',  ( 40.34137639590981905, 24.72187500034139873, 29.30972558990010768 ) ) ;
#13652 = CARTESIAN_POINT ( 'NONE',  ( -3.210462471511496205E-15, 27.35937500034139447, -52.43083105670540789 ) ) ;
#13653 = CARTESIAN_POINT ( 'NONE',  ( 0.000000000000000000, 22.50000000000000000, 102.0000000000000142 ) ) ;
#13654 = CARTESIAN_POINT ( 'NONE',  ( -49.86468353124999453, 34.02187500034140299, 16.20201782572377169 ) ) ;
#13655 = CARTESIAN_POINT ( 'NONE',  ( 3.749999999999932943, 40.00000000000000711, -6.495190528383318451 ) ) ;
#13656 = CARTESIAN_POINT ( 'NONE',  ( 30.81806926056964002, 42.55937500034139020, 42.41743335407647209 ) ) ;
#13657 = CARTESIAN_POINT ( 'NONE',  ( 49.86468353124999453, 39.02187500034138878, -16.20201782572376459 ) ) ;
#13658 = CARTESIAN_POINT ( 'NONE',  ( -30.90169943749473802, 44.30000000000001137, 42.53254041760200721 ) ) ;
#13659 = EDGE_LOOP ( 'NONE', ( #14843, #11627, #10154 ) ) ;
#13660 = AXIS2_PLACEMENT_3D ( 'NONE', #8658, #16227, #14635 ) ;
#13661 = CARTESIAN_POINT ( 'NONE',  ( 30.81806926056962936, 41.15937500034139873, -42.41743335407646498 ) ) ;
#13662 = ORIENTED_EDGE ( 'NONE', *, *, #7579, .F. ) ;
#13663 = EDGE_CURVE ( 'NONE', #9685, #10949, #11187, .T. ) ;
#13664 = CARTESIAN_POINT ( 'NONE',  ( -15.45084971874736368, 22.18125000068279817, 47.55282581475768211 ) ) ;
#13665 = ORIENTED_EDGE ( 'NONE', *, *, #4694, .F. ) ;
#13666 = ADVANCED_FACE ( 'NONE', ( #3061, #4323 ), #14602, .T. ) ;
#13667 = DIRECTION ( 'NONE',  ( 0.8090169943749505599, -0.5877852522924688072, -0.000000000000000000 ) ) ;
#13668 = CARTESIAN_POINT ( 'NONE',  ( -15.40903463028480580, 48.32187500034140015, 47.42413220539094709 ) ) ;
#13669 = CARTESIAN_POINT ( 'NONE',  ( 16.48898053797764973, 28.38332565970932819, 102.0000000000000142 ) ) ;
#13671 = ADVANCED_FACE ( 'NONE', ( #4402 ), #5502, .T. ) ;
#13670 = AXIS2_PLACEMENT_3D ( 'NONE', #212, #7867, #14414 ) ;
#13672 = CARTESIAN_POINT ( 'NONE',  ( -15.40903463028481646, 23.52187500034139944, -47.42413220539093999 ) ) ;
#13673 = CARTESIAN_POINT ( 'NONE',  ( 15.45084971874736723, 31.18125000068279817, -47.55282581475768211 ) ) ;
#13674 = CARTESIAN_POINT ( 'NONE',  ( 49.86468353125000164, 34.92187500034140157, -6.106662507704105588E-15 ) ) ;
#13675 = CARTESIAN_POINT ( 'NONE',  ( 0.000000000000000000, 45.07596123493892293, 92.05189185291139609 ) ) ;
#13676 = CARTESIAN_POINT ( 'NONE',  ( -49.86468353124999453, 37.82187500034139305, -16.20201782572375393 ) ) ;
#13677 = CARTESIAN_POINT ( 'NONE',  ( -40.45084971874737789, 41.58125000068280031, -29.38926261462365730 ) ) ;
#13678 = EDGE_LOOP ( 'NONE', ( #5005, #14371 ) ) ;
#13679 = ORIENTED_EDGE ( 'NONE', *, *, #5927, .F. ) ;
#13680 = VECTOR ( 'NONE', #11812, 1000.000000000000000 ) ;
#13681 = ORIENTED_EDGE ( 'NONE', *, *, #12976, .F. ) ;
#13682 = CARTESIAN_POINT ( 'NONE',  ( 0.000000000000000000, 193.4213562373095385, 0.000000000000000000 ) ) ;
#13683 = CARTESIAN_POINT ( 'NONE',  ( 6.123233995736766085E-15, 50.00000000000000000, -50.00000000000000000 ) ) ;
#13684 =( BOUNDED_CURVE ( )  B_SPLINE_CURVE ( 3, ( #9045, #14100, #7875, #1555 ),
 .UNSPECIFIED., .F., .F. ) 
 B_SPLINE_CURVE_WITH_KNOTS ( ( 4, 4 ),
 ( 0.000000000000000000, 1.570796326794896780 ),
 .UNSPECIFIED. ) 
 CURVE ( )  GEOMETRIC_REPRESENTATION_ITEM ( )  RATIONAL_B_SPLINE_CURVE ( ( 1.000000000000000000, 0.8047378541243649375, 0.8047378541243649375, 1.000000000000000000 ) ) 
 REPRESENTATION_ITEM ( '' )  );
#13685 = CARTESIAN_POINT ( 'NONE',  ( 0.000000000000000000, 20.00000000000000355, 0.000000000000000000 ) ) ;
#13686 = CARTESIAN_POINT ( 'NONE',  ( -30.81806926056962226, 40.15937500034139163, 42.41743335407647919 ) ) ;
#13687 = CARTESIAN_POINT ( 'NONE',  ( -49.86468353124999453, 43.95937500034138878, 16.20201782572377169 ) ) ;
#13688 = CARTESIAN_POINT ( 'NONE',  ( 7.919222016226809657, 25.44874571845315359, -50.00000000000000000 ) ) ;
#13689 = DIRECTION ( 'NONE',  ( 0.000000000000000000, 0.000000000000000000, 1.000000000000000000 ) ) ;
#13690 =( NAMED_UNIT ( * ) PLANE_ANGLE_UNIT ( ) SI_UNIT ( $, .RADIAN. ) );
#13691 = VECTOR ( 'NONE', #15676, 1000.000000000000114 ) ;
#13693 = CARTESIAN_POINT ( 'NONE',  ( 17.50000000000000000, 22.50000000000000355, 102.0000000000000142 ) ) ;
#13692 = VECTOR ( 'NONE', #6683, 1000.000000000000000 ) ;
#13694 = CARTESIAN_POINT ( 'NONE',  ( 50.00000000000000711, 40.89999999999999858, 16.24598481164530739 ) ) ;
#13695 = PLANE ( 'NONE',  #13341 ) ;
#13696 = VERTEX_POINT ( 'NONE', #14438 ) ;
#13697 = CARTESIAN_POINT ( 'NONE',  ( -30.81806926056962226, 26.15937500034139163, 42.41743335407647919 ) ) ;
#13698 = ORIENTED_EDGE ( 'NONE', *, *, #14806, .F. ) ;
#13699 = ORIENTED_EDGE ( 'NONE', *, *, #2766, .T. ) ;
#13700 = EDGE_LOOP ( 'NONE', ( #6176, #3782, #5405, #1085 ) ) ;
#13701 = CARTESIAN_POINT ( 'NONE',  ( 40.45084971874737789, 36.58125000068280031, 29.38926261462365375 ) ) ;
#13702 = CIRCLE ( 'NONE', #9200, 14.08089297201391155 ) ;
#13703 = AXIS2_PLACEMENT_3D ( 'NONE', #7310, #9717, #14770 ) ;
#13704 = DIRECTION ( 'NONE',  ( 0.5877852522924688072, 0.8090169943749505599, 0.000000000000000000 ) ) ;
#13705 = CARTESIAN_POINT ( 'NONE',  ( 7.977241335952203194, 17.31698729810786475, 101.0000000000000000 ) ) ;
#13706 = CIRCLE ( 'NONE', #5514, 100.0000000000000000 ) ;
#13707 = ORIENTED_EDGE ( 'NONE', *, *, #16030, .F. ) ;
#13708 = LINE ( 'NONE', #8552, #6785 ) ;
#13709 = CARTESIAN_POINT ( 'NONE',  ( -16.45433951800529826, 21.27333336793995144, 102.0000000000000142 ) ) ;
#13710 = CARTESIAN_POINT ( 'NONE',  ( 2.978552182361884590E-14, 47.28125000068279604, -50.00000000000000000 ) ) ;
#13711 = CARTESIAN_POINT ( 'NONE',  ( 9.227956911499398113E-15, 102.0000000000000142, -1.913737646857611713E-14 ) ) ;
#13712 = EDGE_CURVE ( 'NONE', #10597, #12892, #10473, .T. ) ;
#13713 = CARTESIAN_POINT ( 'NONE',  ( -20.00000000000000355, 307.0000000000000568, -2.499999999999998668 ) ) ;
#13714 = DIRECTION ( 'NONE',  ( -0.000000000000000000, 1.000000000000000000, -0.000000000000000000 ) ) ;
#13715 = LINE ( 'NONE', #11549, #1700 ) ;
#13716 = CARTESIAN_POINT ( 'NONE',  ( 50.00000000000000000, 46.78125000068279604, -6.123233995736766085E-15 ) ) ;
#13717 = CYLINDRICAL_SURFACE ( 'NONE', #12132, 50.00000000000000000 ) ;
#13718 = AXIS2_PLACEMENT_3D ( 'NONE', #9558, #6909, #15946 ) ;
#13719 = CARTESIAN_POINT ( 'NONE',  ( 50.00000000000000000, 29.00000000000000000, -6.123233995736766085E-15 ) ) ;
#13720 = FACE_OUTER_BOUND ( 'NONE', #4660, .T. ) ;
#13721 = DIRECTION ( 'NONE',  ( 0.000000000000000000, 0.000000000000000000, 1.000000000000000000 ) ) ;
#13723 = EDGE_CURVE ( 'NONE', #12134, #11385, #6627, .T. ) ;
#13722 = VECTOR ( 'NONE', #15937, 1000.000000000000000 ) ;
#13724 = EDGE_CURVE ( 'NONE', #9639, #1788, #13049, .T. ) ;
#13725 = CARTESIAN_POINT ( 'NONE',  ( -40.34137639590981905, 45.65937500034139873, -29.30972558990011478 ) ) ;
#13726 = ORIENTED_EDGE ( 'NONE', *, *, #41, .F. ) ;
#13727 = CARTESIAN_POINT ( 'NONE',  ( -40.34137639590981195, 26.05937500034139731, 29.30972558990012189 ) ) ;
#13728 = EDGE_CURVE ( 'NONE', #6657, #9682, #11881, .T. ) ;
#13729 = EDGE_LOOP ( 'NONE', ( #16170, #5205, #1802, #3196 ) ) ;
#13730 = CARTESIAN_POINT ( 'NONE',  ( 15.45084971874736723, 49.39999999999999858, -47.55282581475768211 ) ) ;
#13731 = CARTESIAN_POINT ( 'NONE',  ( 49.86468353124999453, 36.95937500034139589, -16.20201782572376459 ) ) ;
#13732 = EDGE_CURVE ( 'NONE', #6085, #8525, #557, .T. ) ;
#13733 = CARTESIAN_POINT ( 'NONE',  ( -3.111920190527341144E-15, 27.50000000000000000, -50.00000000000000000 ) ) ;
#13734 = CARTESIAN_POINT ( 'NONE',  ( -8.880528407616480990, 25.91118970470954963, 101.0000000000000000 ) ) ;
#13735 = DIRECTION ( 'NONE',  ( -0.6691306063588569053, -0.7431448254773954654, 0.000000000000000000 ) ) ;
#13736 = CARTESIAN_POINT ( 'NONE',  ( 2.978552182361884590E-14, 47.28125000068279604, -50.00000000000000000 ) ) ;
#13737 = CARTESIAN_POINT ( 'NONE',  ( -30.81806926056962226, 20.22187500034139163, 42.41743335407647919 ) ) ;
#13738 = CARTESIAN_POINT ( 'NONE',  ( 30.81806926056964002, 30.55937500034139731, 42.41743335407646498 ) ) ;
#13739 = CARTESIAN_POINT ( 'NONE',  ( 7.580410092413973011, 99.32916037694960210, 5.000000000000000000 ) ) ;
#13740 = CARTESIAN_POINT ( 'NONE',  ( -15.40903463028480580, 32.32187500034139305, 47.42413220539094709 ) ) ;
#13741 = DIRECTION ( 'NONE',  ( -0.000000000000000000, 1.000000000000000000, -0.000000000000000000 ) ) ;
#13742 = CARTESIAN_POINT ( 'NONE',  ( 49.99999999999999289, 39.10000000000000853, -16.24598481164532160 ) ) ;
#13743 = CARTESIAN_POINT ( 'NONE',  ( -15.40903463028481646, 41.45937500034140299, -47.42413220539093999 ) ) ;
#13744 = CARTESIAN_POINT ( 'NONE',  ( 15.40903463028481113, 35.32187500034139305, -47.42413220539094709 ) ) ;
#13745 = CARTESIAN_POINT ( 'NONE',  ( 15.45084971874737789, 42.60000000000000142, 47.55282581475767500 ) ) ;
#13746 = CIRCLE ( 'NONE', #11897, 2.000000000000000000 ) ;
#13747 = ORIENTED_EDGE ( 'NONE', *, *, #10543, .F. ) ;
#13748 = CARTESIAN_POINT ( 'NONE',  ( 49.86468353125001585, 42.75937500034138594, 16.20201782572375038 ) ) ;
#13749 = ORIENTED_EDGE ( 'NONE', *, *, #10082, .F. ) ;
#13750 = CARTESIAN_POINT ( 'NONE',  ( -50.00000000000000000, 21.78125000068279959, 0.000000000000000000 ) ) ;
#13751 = DIRECTION ( 'NONE',  ( -0.3090169943749573878, 0.9510565162951503115, 0.000000000000000000 ) ) ;
#13752 = LINE ( 'NONE', #12182, #8119 ) ;
#13753 = CIRCLE ( 'NONE', #3418, 50.00000000000000000 ) ;
#13754 = CARTESIAN_POINT ( 'NONE',  ( -49.86468353125000164, 43.92187500034140157, 0.000000000000000000 ) ) ;
#13755 = CARTESIAN_POINT ( 'NONE',  ( 40.45084971874737789, 30.80000000000000071, 29.38926261462365375 ) ) ;
#13756 = CARTESIAN_POINT ( 'NONE',  ( -30.81806926056962226, 22.22187500034139163, 42.41743335407647919 ) ) ;
#13757 =( BOUNDED_CURVE ( )  B_SPLINE_CURVE ( 3, ( #1848, #5689, #9183, #8182 ),
 .UNSPECIFIED., .F., .F. ) 
 B_SPLINE_CURVE_WITH_KNOTS ( ( 4, 4 ),
 ( 4.523772594209285458, 4.712388980384689674 ),
 .UNSPECIFIED. ) 
 CURVE ( )  GEOMETRIC_REPRESENTATION_ITEM ( )  RATIONAL_B_SPLINE_CURVE ( ( 1.000000000000000000, 0.9970375182503885547, 0.9970375182503885547, 1.000000000000000000 ) ) 
 REPRESENTATION_ITEM ( '' )  );
#13758 = CARTESIAN_POINT ( 'NONE',  ( 49.99999999999999289, 24.88125000068279746, -16.24598481164532160 ) ) ;
#13759 = CARTESIAN_POINT ( 'NONE',  ( 30.81806926056962936, 37.22187500034139873, -42.41743335407647209 ) ) ;
#13760 = CARTESIAN_POINT ( 'NONE',  ( -29.01527194596337011, 282.0655843567852799, -11.51527194596495107 ) ) ;
#13761 = CARTESIAN_POINT ( 'NONE',  ( 40.34137639590981905, 34.72187500034139873, 29.30972558990010768 ) ) ;
#13762 = CARTESIAN_POINT ( 'NONE',  ( -15.45084971874736368, 42.18125000068279462, 47.55282581475768211 ) ) ;
#13763 = EDGE_LOOP ( 'NONE', ( #12316, #16359, #10485 ) ) ;
#13764 = ORIENTED_EDGE ( 'NONE', *, *, #3788, .T. ) ;
#13765 = ORIENTED_EDGE ( 'NONE', *, *, #13129, .F. ) ;
#13766 = EDGE_CURVE ( 'NONE', #12958, #13340, #3639, .T. ) ;
#13767 = CARTESIAN_POINT ( 'NONE',  ( -50.00000000000000000, 32.00000000000000000, 0.000000000000000000 ) ) ;
#13768 = DIRECTION ( 'NONE',  ( 0.000000000000000000, 1.000000000000000000, 0.000000000000000000 ) ) ;
#13769 = DIRECTION ( 'NONE',  ( 0.1045284632676436315, 0.9945218953682742891, 0.000000000000000000 ) ) ;
#13770 = CARTESIAN_POINT ( 'NONE',  ( -50.00000000000000000, 23.78125000068279959, 0.000000000000000000 ) ) ;
#13771 = CARTESIAN_POINT ( 'NONE',  ( -30.81806926056962226, 34.15937500034139163, 42.41743335407647919 ) ) ;
#13772 = CARTESIAN_POINT ( 'NONE',  ( -49.86468353124999453, 41.75937500034139305, -16.20201782572375393 ) ) ;
#13773 = DIRECTION ( 'NONE',  ( 0.000000000000000000, 0.000000000000000000, -1.000000000000000000 ) ) ;
#13774 = AXIS2_PLACEMENT_3D ( 'NONE', #5581, #10566, #6746 ) ;
#13775 = CARTESIAN_POINT ( 'NONE',  ( 0.000000000000000000, 28.00000000000000355, 0.000000000000000000 ) ) ;
#13776 = LINE ( 'NONE', #15106, #13227 ) ;
#13777 = CARTESIAN_POINT ( 'NONE',  ( -50.00000000000000000, 49.89062500034140157, 0.000000000000000000 ) ) ;
#13778 = ORIENTED_EDGE ( 'NONE', *, *, #7162, .T. ) ;
#13779 = CARTESIAN_POINT ( 'NONE',  ( -15.40903463028480580, 26.25937500034140015, 47.42413220539094709 ) ) ;
#13780 = DIRECTION ( 'NONE',  ( 0.3420201433256697121, -0.6644630243886754384, -0.6644630243886734400 ) ) ;
#13781 = ORIENTED_EDGE ( 'NONE', *, *, #4819, .T. ) ;
#13782 = ORIENTED_EDGE ( 'NONE', *, *, #13016, .F. ) ;
#13783 =( BOUNDED_CURVE ( )  B_SPLINE_CURVE ( 2, ( #11856, #4302, #9366, #10695, #458, #12014, #6961, #10622, #6043, #14657, #15999, #781, #5873 ),
 .UNSPECIFIED., .F., .T. ) 
 B_SPLINE_CURVE_WITH_KNOTS ( ( 3, 2, 2, 2, 2, 2, 3 ),
 ( 0.5166666666666667185, 0.5200000000000000178, 0.5266666666666666163, 0.5333333333333333259, 0.5400000000000000355, 0.5466666666666666341, 0.5500000000000000444 ),
 .UNSPECIFIED. ) 
 CURVE ( )  GEOMETRIC_REPRESENTATION_ITEM ( )  RATIONAL_B_SPLINE_CURVE ( ( 0.9755282581475768211, 0.9755282581475771542, 1.000000000000000000, 0.9510565162951535312, 1.000000000000000000, 0.9510565162951535312, 1.000000000000000000, 0.9510565162951535312, 1.000000000000000000, 0.9510565162951535312, 1.000000000000000000, 0.9755282581475763770, 0.9755282581475768211 ) ) 
 REPRESENTATION_ITEM ( '' )  );
#13784 = CARTESIAN_POINT ( 'NONE',  ( 30.90169943749475578, 38.48125000068279178, 42.53254041760200010 ) ) ;
#13785 = AXIS2_PLACEMENT_3D ( 'NONE', #971, #13607, #10958 ) ;
#13786 = DIRECTION ( 'NONE',  ( -0.000000000000000000, -1.000000000000000000, -0.000000000000000000 ) ) ;
#13787 = VERTEX_POINT ( 'NONE', #15620 ) ;
#13788 = CARTESIAN_POINT ( 'NONE',  ( 50.00000000000000000, 38.78125000068279604, -6.123233995736766085E-15 ) ) ;
#13789 = LINE ( 'NONE', #3825, #8229 ) ;
#13790 = DIRECTION ( 'NONE',  ( -1.000000000000000000, 0.000000000000000000, -1.734723475976807094E-17 ) ) ;
#13791 = DIRECTION ( 'NONE',  ( 0.8090169943749505599, -0.5877852522924689183, 0.000000000000000000 ) ) ;
#13792 = CARTESIAN_POINT ( 'NONE',  ( -5.000000000000000000, 100.8332763660826572, -11.66170349082880442 ) ) ;
#13793 = DIRECTION ( 'NONE',  ( 0.000000000000000000, 0.000000000000000000, -1.000000000000000000 ) ) ;
#13794 = DIRECTION ( 'NONE',  ( -0.5877852522924797984, 0.8090169943749424553, 0.000000000000000000 ) ) ;
#13795 =( LENGTH_UNIT ( ) NAMED_UNIT ( * ) SI_UNIT ( .MILLI., .METRE. ) );
#13796 = DIRECTION ( 'NONE',  ( 0.5877852522924688072, 0.8090169943749505599, 0.000000000000000000 ) ) ;
#13797 = CARTESIAN_POINT ( 'NONE',  ( 30.90169943749475578, 48.48125000068279888, 42.53254041760200010 ) ) ;
#13798 = CARTESIAN_POINT ( 'NONE',  ( 7.919222016226940219, 21.44874571845316069, -49.99999999999996447 ) ) ;
#13799 = ADVANCED_FACE ( 'NONE', ( #4246, #9312 ), #14365, .T. ) ;
#13800 = CARTESIAN_POINT ( 'NONE',  ( 30.90169943749475578, 24.69999999999999929, 42.53254041760200010 ) ) ;
#13801 = EDGE_CURVE ( 'NONE', #10305, #6366, #7147, .T. ) ;
#13802 = LINE ( 'NONE', #1245, #13183 ) ;
#13803 = CARTESIAN_POINT ( 'NONE',  ( 16.79799753235259985, 27.43226914341417810, 101.0000000000000000 ) ) ;
#13804 = CARTESIAN_POINT ( 'NONE',  ( 15.40903463028481113, 43.25937500034139305, -47.42413220539094709 ) ) ;
#13805 = EDGE_LOOP ( 'NONE', ( #7401, #1895, #4814, #3319 ) ) ;
#13806 = ORIENTED_EDGE ( 'NONE', *, *, #10710, .T. ) ;
#13807 = LINE ( 'NONE', #2747, #3907 ) ;
#13808 = CARTESIAN_POINT ( 'NONE',  ( 49.86468353124999453, 30.95937500034139944, -16.20201782572376459 ) ) ;
#13809 = DIRECTION ( 'NONE',  ( -1.000000000000000000, 0.000000000000000000, 0.000000000000000000 ) ) ;
#13811 = EDGE_CURVE ( 'NONE', #11147, #5908, #9962, .T. ) ;
#13810 = DIRECTION ( 'NONE',  ( 0.000000000000000000, 0.000000000000000000, 1.000000000000000000 ) ) ;
#13812 = CARTESIAN_POINT ( 'NONE',  ( 45.74278786629302118, 25.00000000000000000, -19.85154960931340185 ) ) ;
#13813 = CARTESIAN_POINT ( 'NONE',  ( 2.600676159226420495E-13, 31.28125000068279604, -49.99999999999999289 ) ) ;
#13814 = CARTESIAN_POINT ( 'NONE',  ( 30.81806926056962936, 23.22187500034139163, -42.41743335407647209 ) ) ;
#13815 = CARTESIAN_POINT ( 'NONE',  ( -15.40903463028481646, 25.45937500034139589, -47.42413220539093999 ) ) ;
#13816 = CARTESIAN_POINT ( 'NONE',  ( -4.678013043399745108, 44.50832101651058537, 101.0000000000000000 ) ) ;
#13817 = CARTESIAN_POINT ( 'NONE',  ( 9.631387414534489405E-15, 38.42187500034139447, 52.43083105670540789 ) ) ;
#13818 = FACE_OUTER_BOUND ( 'NONE', #7802, .T. ) ;
#13819 = CARTESIAN_POINT ( 'NONE',  ( -3.219174618344376363E-15, 35.50000000000000000, -52.57311121191334990 ) ) ;
#13820 = CARTESIAN_POINT ( 'NONE',  ( -40.34137639590981905, 39.65937500034139873, -29.30972558990011478 ) ) ;
#13821 = CARTESIAN_POINT ( 'NONE',  ( -15.40903463028480580, 34.32187500034139305, 47.42413220539094709 ) ) ;
#13822 = CARTESIAN_POINT ( 'NONE',  ( 15.45084971874736723, 47.40000000000000568, -47.55282581475768211 ) ) ;
#13823 = ORIENTED_EDGE ( 'NONE', *, *, #11682, .T. ) ;
#13824 = EDGE_CURVE ( 'NONE', #12158, #1479, #7096, .T. ) ;
#13825 = CARTESIAN_POINT ( 'NONE',  ( -40.34137639590981905, 37.65937500034139873, -29.30972558990011478 ) ) ;
#13826 = VERTEX_POINT ( 'NONE', #10881 ) ;
#13827 = ORIENTED_EDGE ( 'NONE', *, *, #10633, .T. ) ;
#13828 = CARTESIAN_POINT ( 'NONE',  ( 50.00000000000000711, 24.68125000068279462, 16.24598481164530739 ) ) ;
#13829 = CARTESIAN_POINT ( 'NONE',  ( 6.123233995736766085E-15, 20.00000000000000355, -50.00000000000000000 ) ) ;
#13830 = CARTESIAN_POINT ( 'NONE',  ( -3.210462471511496205E-15, 25.42187500034139092, -52.43083105670540789 ) ) ;
#13831 = DIRECTION ( 'NONE',  ( 0.000000000000000000, 0.000000000000000000, -1.000000000000000000 ) ) ;
#13832 = CARTESIAN_POINT ( 'NONE',  ( 40.34137639590981195, 45.12187500034139731, -29.30972558990011834 ) ) ;
#13833 = CARTESIAN_POINT ( 'NONE',  ( -12.83864924538561780, 33.38715533906339061, 101.6666710451724214 ) ) ;
#13834 = CARTESIAN_POINT ( 'NONE',  ( 50.00000000000000711, 46.90000000000000568, 16.24598481164530739 ) ) ;
#13835 = EDGE_CURVE ( 'NONE', #4080, #8192, #6828, .T. ) ;
#13836 = CARTESIAN_POINT ( 'NONE',  ( -30.90169943749474868, 27.48125000068279888, -42.53254041760200721 ) ) ;
#13837 = CARTESIAN_POINT ( 'NONE',  ( -30.90169943749474513, 45.70000000000000284, -42.53254041760200721 ) ) ;
#13838 = CARTESIAN_POINT ( 'NONE',  ( -15.40903463028480580, 32.32187500034139305, 47.42413220539094709 ) ) ;
#13839 = CARTESIAN_POINT ( 'NONE',  ( -25.75618375337248622, 283.9316295015380547, -8.256183753375490042 ) ) ;
#13840 = CARTESIAN_POINT ( 'NONE',  ( 49.86468353125001585, 38.82187500034140015, 16.20201782572375038 ) ) ;
#13841 = CARTESIAN_POINT ( 'NONE',  ( 2.600676159226421000E-13, 33.28125000068279604, -49.99999999999999289 ) ) ;
#13842 = ORIENTED_EDGE ( 'NONE', *, *, #5410, .F. ) ;
#13843 = VERTEX_POINT ( 'NONE', #886 ) ;
#13844 = APPLICATION_CONTEXT ( 'automotive_design' ) ;
#13845 = CARTESIAN_POINT ( 'NONE',  ( 30.27664397204019409, 40.00000000000000711, -26.14048258526078072 ) ) ;
#13846 = DIRECTION ( 'NONE',  ( -1.000000000000000000, 0.000000000000000000, -0.000000000000000000 ) ) ;
#13847 = CARTESIAN_POINT ( 'NONE',  ( -16.50000000000000711, 22.50000000000000000, 102.0000000000000142 ) ) ;
#13848 = CARTESIAN_POINT ( 'NONE',  ( 0.000000000000000000, 20.00000000000000355, 0.000000000000000000 ) ) ;
#13849 = CARTESIAN_POINT ( 'NONE',  ( 30.81806926056962936, 29.15937500034139518, -42.41743335407647209 ) ) ;
#13850 = ADVANCED_FACE ( 'NONE', ( #12208 ), #12369, .F. ) ;
#13851 = LINE ( 'NONE', #16353, #3709 ) ;
#13852 = CARTESIAN_POINT ( 'NONE',  ( -15.40903463028480580, 44.32187500034140015, 47.42413220539094709 ) ) ;
#13853 = SURFACE_STYLE_FILL_AREA ( #6313 ) ;
#13854 = DIRECTION ( 'NONE',  ( 6.938893903907231459E-18, -1.000000000000000000, -5.551115123125782702E-17 ) ) ;
#13855 = CARTESIAN_POINT ( 'NONE',  ( -30.27664397204038593, 40.00000000000000711, 26.14048258526057467 ) ) ;
#13856 = FACE_OUTER_BOUND ( 'NONE', #11988, .T. ) ;
#13857 = ORIENTED_EDGE ( 'NONE', *, *, #4003, .T. ) ;
#13858 = AXIS2_PLACEMENT_3D ( 'NONE', #8384, #9561, #735 ) ;
#13859 = CARTESIAN_POINT ( 'NONE',  ( 49.86468353125000164, 24.85937500034139802, -6.106662507704105588E-15 ) ) ;
#13860 = ORIENTED_EDGE ( 'NONE', *, *, #3362, .T. ) ;
#13861 = EDGE_LOOP ( 'NONE', ( #8713, #5723, #14952, #744 ) ) ;
#13862 = ORIENTED_EDGE ( 'NONE', *, *, #2345, .T. ) ;
#13863 = ORIENTED_EDGE ( 'NONE', *, *, #2842, .T. ) ;
#13864 = DIRECTION ( 'NONE',  ( -0.6691306063588569053, -0.7431448254773954654, 0.000000000000000000 ) ) ;
#13865 = LINE ( 'NONE', #7561, #2244 ) ;
#13866 = CARTESIAN_POINT ( 'NONE',  ( 7.919222016226758143, 38.33250428222964246, 50.00000000000000711 ) ) ;
#13867 = CARTESIAN_POINT ( 'NONE',  ( -49.99999999999999289, 37.90000000000000568, -16.24598481164531449 ) ) ;
#13868 = CARTESIAN_POINT ( 'NONE',  ( -40.34137639590981905, 49.65937500034139873, -29.30972558990011478 ) ) ;
#13869 = CARTESIAN_POINT ( 'NONE',  ( 9.574901606694759531E-15, 52.00000000000001421, -2.191293403013901479E-14 ) ) ;
#13870 = CARTESIAN_POINT ( 'NONE',  ( -3.111920190527341144E-15, 27.28125000068279604, -50.00000000000000000 ) ) ;
#13871 = DIRECTION ( 'NONE',  ( 0.5000000000000041078, 0.000000000000000000, 0.8660254037844362651 ) ) ;
#13873 = DIRECTION ( 'NONE',  ( 0.000000000000000000, 0.000000000000000000, -1.000000000000000000 ) ) ;
#13872 = VECTOR ( 'NONE', #13067, 1000.000000000000000 ) ;
#13874 = FILL_AREA_STYLE ('',( #5173 ) ) ;
#13875 = CARTESIAN_POINT ( 'NONE',  ( -3.219174618344376363E-15, 45.28125000068279604, -52.57311121191334990 ) ) ;
#13876 = CARTESIAN_POINT ( 'NONE',  ( 40.45084971874737079, 44.98125000068279888, -29.38926261462366440 ) ) ;
#13877 = CARTESIAN_POINT ( 'NONE',  ( 49.99999999999999289, 23.10000000000000497, -16.24598481164532160 ) ) ;
#13878 = CYLINDRICAL_SURFACE ( 'NONE', #1763, 5.000000000000000888 ) ;
#13879 = LINE ( 'NONE', #10989, #146 ) ;
#13880 =( BOUNDED_CURVE ( )  B_SPLINE_CURVE ( 2, ( #13736, #5113, #12573, #16315, #12498, #1091, #11257, #4950, #7502, #177, #15218, #1420, #7672 ),
 .UNSPECIFIED., .F., .T. ) 
 B_SPLINE_CURVE_WITH_KNOTS ( ( 3, 2, 2, 2, 2, 2, 3 ),
 ( 0.08333333333333334259, 0.08666666666666666963, 0.09333333333333333759, 0.1000000000000000056, 0.1066666666666666735, 0.1133333333333333276, 0.1166666666666666685 ),
 .UNSPECIFIED. ) 
 CURVE ( )  GEOMETRIC_REPRESENTATION_ITEM ( )  RATIONAL_B_SPLINE_CURVE ( ( 0.9755282581475768211, 0.9755282581475768211, 1.000000000000000000, 0.9510565162951535312, 1.000000000000000000, 0.9510565162951535312, 1.000000000000000000, 0.9510565162951535312, 1.000000000000000000, 0.9510565162951535312, 1.000000000000000000, 0.9755282581475767101, 0.9755282581475768211 ) ) 
 REPRESENTATION_ITEM ( '' )  );
#13881 = CARTESIAN_POINT ( 'NONE',  ( -30.81806926056963292, 41.55937500034139731, -42.41743335407647209 ) ) ;
#13882 = ORIENTED_EDGE ( 'NONE', *, *, #8946, .F. ) ;
#13883 = ORIENTED_EDGE ( 'NONE', *, *, #9357, .T. ) ;
#13884 = FACE_OUTER_BOUND ( 'NONE', #4965, .T. ) ;
#13885 = CARTESIAN_POINT ( 'NONE',  ( 15.40903463028481113, 27.25937500034139660, -47.42413220539094709 ) ) ;
#13886 = CARTESIAN_POINT ( 'NONE',  ( 7.919222016226940219, 33.44874571845316069, -49.99999999999996447 ) ) ;
#13887 = LINE ( 'NONE', #6684, #3343 ) ;
#13888 = CARTESIAN_POINT ( 'NONE',  ( 48.35726954556789536, 24.99999999999999645, -12.16803787670825265 ) ) ;
#13889 = CARTESIAN_POINT ( 'NONE',  ( 30.81806926056964002, 36.62187500034139731, 42.41743335407646498 ) ) ;
#13890 = LINE ( 'NONE', #6513, #11850 ) ;
#13891 = CARTESIAN_POINT ( 'NONE',  ( 49.86468353125001585, 22.82187500034138949, 16.20201782572375038 ) ) ;
#13892 = CARTESIAN_POINT ( 'NONE',  ( 9.631387414534489405E-15, 20.35937500034139092, 52.43083105670540789 ) ) ;
#13893 = CARTESIAN_POINT ( 'NONE',  ( 15.45084971874736723, 43.39999999999999858, -47.55282581475768211 ) ) ;
#13894 = CARTESIAN_POINT ( 'NONE',  ( 30.81806926056964002, 34.62187500034139731, 42.41743335407646498 ) ) ;
#13895 = CARTESIAN_POINT ( 'NONE',  ( 0.000000000000000000, 50.00000000000000000, 0.000000000000000000 ) ) ;
#13896 = AXIS2_PLACEMENT_3D ( 'NONE', #10496, #4184, #11813 ) ;
#13897 = CARTESIAN_POINT ( 'NONE',  ( 50.00000000000000711, 32.89999999999999147, 16.24598481164530739 ) ) ;
#13898 = CARTESIAN_POINT ( 'NONE',  ( -49.86468353124999453, 37.75937500034140015, -16.20201782572375393 ) ) ;
#13899 = CARTESIAN_POINT ( 'NONE',  ( 49.86468353124999453, 31.02187500034139234, -16.20201782572376459 ) ) ;
#13900 = CARTESIAN_POINT ( 'NONE',  ( 50.00000000000000711, 44.90000000000000568, 16.24598481164530739 ) ) ;
#13901 = ORIENTED_EDGE ( 'NONE', *, *, #5959, .T. ) ;
#13902 = ORIENTED_EDGE ( 'NONE', *, *, #1732, .F. ) ;
#13903 = CARTESIAN_POINT ( 'NONE',  ( 40.34137639590981195, 37.05937500034139731, -29.30972558990011834 ) ) ;
#13904 = ORIENTED_EDGE ( 'NONE', *, *, #7058, .T. ) ;
#13905 = ORIENTED_EDGE ( 'NONE', *, *, #2766, .F. ) ;
#13906 = CARTESIAN_POINT ( 'NONE',  ( 1.293669679204937499E-13, 41.50000000000000000, -50.00000000000000000 ) ) ;
#13907 = CARTESIAN_POINT ( 'NONE',  ( -49.86468353125000164, 47.85937500034139447, 0.000000000000000000 ) ) ;
#13908 = CIRCLE ( 'NONE', #7546, 17.50000000000000000 ) ;
#13909 = FACE_BOUND ( 'NONE', #9487, .T. ) ;
#13910 = CARTESIAN_POINT ( 'NONE',  ( -49.86468353124999453, 21.82187500034139305, -16.20201782572375393 ) ) ;
#13911 = CARTESIAN_POINT ( 'NONE',  ( 0.000000000000000000, 22.50000000000000000, 102.0000000000000142 ) ) ;
#13912 = CARTESIAN_POINT ( 'NONE',  ( 9.631387414534489405E-15, 42.42187500034140157, 52.43083105670540789 ) ) ;
#13913 = CARTESIAN_POINT ( 'NONE',  ( -1.240322475938754499E-13, 40.50000000000000000, 50.00000000000000000 ) ) ;
#13914 = EDGE_CURVE ( 'NONE', #10702, #2271, #8376, .T. ) ;
#13915 = CARTESIAN_POINT ( 'NONE',  ( -40.45084971874737789, 47.80000000000000426, -29.38926261462365730 ) ) ;
#13916 = CARTESIAN_POINT ( 'NONE',  ( 30.90169943749474157, 29.08125000068280031, -42.53254041760200721 ) ) ;
#13917 = CARTESIAN_POINT ( 'NONE',  ( -40.34137639590981905, 47.72187500034139873, -29.30972558990011478 ) ) ;
#13918 = CARTESIAN_POINT ( 'NONE',  ( -49.86468353124999453, 35.82187500034139305, -16.20201782572375393 ) ) ;
#13919 = CARTESIAN_POINT ( 'NONE',  ( 0.000000000000000000, 22.50000000000000000, 102.0000000000000142 ) ) ;
#13920 = EDGE_CURVE ( 'NONE', #8386, #14589, #1058, .T. ) ;
#13921 = EDGE_CURVE ( 'NONE', #2225, #2271, #11340, .T. ) ;
#13922 = CARTESIAN_POINT ( 'NONE',  ( 1.790468199911983804, 101.0808929720139275, 9.080892972013892006 ) ) ;
#13923 = ORIENTED_EDGE ( 'NONE', *, *, #2754, .F. ) ;
#13924 = ADVANCED_FACE ( 'NONE', ( #5979 ), #3653, .F. ) ;
#13925 = ORIENTED_EDGE ( 'NONE', *, *, #15396, .T. ) ;
#13926 = CARTESIAN_POINT ( 'NONE',  ( -15.45084971874736368, 32.39999999999999858, 47.55282581475768211 ) ) ;
#13927 = DIRECTION ( 'NONE',  ( 0.000000000000000000, 1.000000000000000000, -0.000000000000000000 ) ) ;
#13928 = CIRCLE ( 'NONE', #6512, 24.08089297201390977 ) ;
#13929 = DIRECTION ( 'NONE',  ( -1.000000000000000000, 0.000000000000000000, 0.000000000000000000 ) ) ;
#13930 = CARTESIAN_POINT ( 'NONE',  ( -49.99999999999999289, 23.68125000068279462, -16.24598481164531449 ) ) ;
#13931 = CARTESIAN_POINT ( 'NONE',  ( -15.40903463028481646, 29.45937500034139589, -47.42413220539093999 ) ) ;
#13932 = CARTESIAN_POINT ( 'NONE',  ( 40.34137639590981195, 43.12187500034139731, -29.30972558990011834 ) ) ;
#13933 =( NAMED_UNIT ( * ) SI_UNIT ( $, .STERADIAN. ) SOLID_ANGLE_UNIT ( ) );
#13934 = CARTESIAN_POINT ( 'NONE',  ( -15.45084971874736368, 40.40000000000000568, 47.55282581475768211 ) ) ;
#13935 = DIRECTION ( 'NONE',  ( -1.000000000000000000, 0.000000000000000000, 0.000000000000000000 ) ) ;
#13936 = CARTESIAN_POINT ( 'NONE',  ( -2.500000000000000000, 242.0000000000000284, 47.99999999999999289 ) ) ;
#13937 = ORIENTED_EDGE ( 'NONE', *, *, #5901, .F. ) ;
#13938 = VECTOR ( 'NONE', #11131, 1000.000000000000000 ) ;
#13939 = CARTESIAN_POINT ( 'NONE',  ( -40.34137639590981905, 27.65937500034139873, -29.30972558990011478 ) ) ;
#13940 = ORIENTED_EDGE ( 'NONE', *, *, #14051, .F. ) ;
#13941 = CARTESIAN_POINT ( 'NONE',  ( -7.919222016226822092, 46.22999571913594963, 50.00000000000000000 ) ) ;
#13942 = VERTEX_POINT ( 'NONE', #12535 ) ;
#13943 = ORIENTED_EDGE ( 'NONE', *, *, #14156, .T. ) ;
#13944 = CARTESIAN_POINT ( 'NONE',  ( 9.189545401991395579, 24.96013318841451678, 101.0000000000000000 ) ) ;
#13945 = EDGE_CURVE ( 'NONE', #15132, #9397, #5814, .T. ) ;
#13946 = FACE_OUTER_BOUND ( 'NONE', #8308, .T. ) ;
#13947 = DIRECTION ( 'NONE',  ( 1.000000000000000000, 0.000000000000000000, 0.000000000000000000 ) ) ;
#13948 = DIRECTION ( 'NONE',  ( 0.000000000000000000, 0.000000000000000000, 1.000000000000000000 ) ) ;
#13949 = CARTESIAN_POINT ( 'NONE',  ( -40.34137639590981195, 48.05937500034139731, 29.30972558990012189 ) ) ;
#13950 = CARTESIAN_POINT ( 'NONE',  ( 9.500222237632415911, 22.00424054664152607, 101.0000000000000000 ) ) ;
#13951 = AXIS2_PLACEMENT_3D ( 'NONE', #6305, #8868, #3804 ) ;
#13952 = AXIS2_PLACEMENT_3D ( 'NONE', #6582, #14114, #5261 ) ;
#13953 = DIRECTION ( 'NONE',  ( 0.000000000000000000, 0.000000000000000000, 1.000000000000000000 ) ) ;
#13954 = CARTESIAN_POINT ( 'NONE',  ( 33.58330087751625825, 35.02991267065631575, -22.31061932477009080 ) ) ;
#13955 = VECTOR ( 'NONE', #6998, 1000.000000000000114 ) ;
#13956 = MECHANICAL_DESIGN_GEOMETRIC_PRESENTATION_REPRESENTATION (  '', ( #11585 ), #1494 ) ;
#13957 = FACE_OUTER_BOUND ( 'NONE', #2397, .T. ) ;
#13958 = CARTESIAN_POINT ( 'NONE',  ( 15.45084971874736723, 39.18125000068280173, -47.55282581475768211 ) ) ;
#13959 = LINE ( 'NONE', #7656, #13991 ) ;
#13960 = AXIS2_PLACEMENT_3D ( 'NONE', #10524, #9275, #8095 ) ;
#13961 = CARTESIAN_POINT ( 'NONE',  ( -49.99999999999999289, 20.09999999999999787, 16.24598481164533226 ) ) ;
#13962 = CARTESIAN_POINT ( 'NONE',  ( -40.34137639590981195, 22.05937500034139731, 29.30972558990012189 ) ) ;
#13963 = VERTEX_POINT ( 'NONE', #1052 ) ;
#13964 = CARTESIAN_POINT ( 'NONE',  ( -49.86468353124999453, 45.75937500034140015, -16.20201782572375393 ) ) ;
#13965 = VERTEX_POINT ( 'NONE', #13532 ) ;
#13966 = AXIS2_PLACEMENT_3D ( 'NONE', #14896, #14811, #676 ) ;
#13967 = VECTOR ( 'NONE', #15944, 1000.000000000000000 ) ;
#13968 = AXIS2_PLACEMENT_3D ( 'NONE', #14956, #748, #5999 ) ;
#13969 = DIRECTION ( 'NONE',  ( -0.000000000000000000, -0.000000000000000000, -1.000000000000000000 ) ) ;
#13970 = DIRECTION ( 'NONE',  ( 0.000000000000000000, -0.000000000000000000, 1.000000000000000000 ) ) ;
#13971 = CARTESIAN_POINT ( 'NONE',  ( 30.81806926056962936, 31.15937500034139518, -42.41743335407647209 ) ) ;
#13972 = ORIENTED_EDGE ( 'NONE', *, *, #7282, .F. ) ;
#13973 = ADVANCED_FACE ( 'NONE', ( #13452 ), #2214, .F. ) ;
#13974 = CARTESIAN_POINT ( 'NONE',  ( -3.991010794631277836, 39.54842293358396432, 92.94258460798921817 ) ) ;
#13975 = CARTESIAN_POINT ( 'NONE',  ( 45.40153297753701622, 25.00000000000000000, -20.62078143446418821 ) ) ;
#13976 = CARTESIAN_POINT ( 'NONE',  ( -40.34137639590981905, 35.72187500034139163, -29.30972558990011478 ) ) ;
#13977 = CARTESIAN_POINT ( 'NONE',  ( 0.000000000000000000, 53.82568851450475478, 65.15972704814865324 ) ) ;
#13978 = VECTOR ( 'NONE', #12503, 1000.000000000000000 ) ;
#13979 = CARTESIAN_POINT ( 'NONE',  ( 49.86468353124999453, 22.95937500034139589, -16.20201782572376104 ) ) ;
#13980 = CARTESIAN_POINT ( 'NONE',  ( -17.28626291527383430, 40.00000000000000711, 18.64048258526052848 ) ) ;
#13981 = CARTESIAN_POINT ( 'NONE',  ( 49.86468353124999453, 37.02187500034138878, -16.20201782572376104 ) ) ;
#13982 = CIRCLE ( 'NONE', #9473, 17.50000000000000000 ) ;
#13983 = CARTESIAN_POINT ( 'NONE',  ( -12.59082374547745076, 33.16401225666594854, 102.0000000000000142 ) ) ;
#13984 = CARTESIAN_POINT ( 'NONE',  ( -3.219174618344376363E-15, 31.50000000000000000, -52.57311121191334990 ) ) ;
#13985 = CARTESIAN_POINT ( 'NONE',  ( -49.86468353125000164, 41.85937500034139447, 0.000000000000000000 ) ) ;
#13986 = CARTESIAN_POINT ( 'NONE',  ( 9.631387414534489405E-15, 34.42187500034138736, 52.43083105670540789 ) ) ;
#13987 = CARTESIAN_POINT ( 'NONE',  ( -3.219174618344376363E-15, 45.49999999999999289, -52.57311121191334990 ) ) ;
#13988 = VERTEX_POINT ( 'NONE', #16024 ) ;
#13989 = EDGE_LOOP ( 'NONE', ( #824, #8992, #9532, #13080 ) ) ;
#13990 = CARTESIAN_POINT ( 'NONE',  ( -49.86468353124999453, 33.95937500034139589, 16.20201782572377169 ) ) ;
#13991 = VECTOR ( 'NONE', #1322, 1000.000000000000000 ) ;
#13992 = ORIENTED_EDGE ( 'NONE', *, *, #6334, .T. ) ;
#13993 = VERTEX_POINT ( 'NONE', #4652 ) ;
#13994 = CARTESIAN_POINT ( 'NONE',  ( -17.28626291527396930, 25.00000000000000355, -18.64048258526039703 ) ) ;
#13996 = CARTESIAN_POINT ( 'NONE',  ( 40.45084971874737789, 20.58125000068280031, 29.38926261462365375 ) ) ;
#13995 = AXIS2_PLACEMENT_3D ( 'NONE', #14430, #6821, #14358 ) ;
#13997 = CARTESIAN_POINT ( 'NONE',  ( 2.500000000000000000, 217.0000000000000284, -44.93050188902856945 ) ) ;
#13998 = CARTESIAN_POINT ( 'NONE',  ( 49.86468353124999453, 21.02187500034139589, -16.20201782572376459 ) ) ;
#13999 = SPHERICAL_SURFACE ( 'NONE', #2001, 5.000000000000000000 ) ;
#14000 = CARTESIAN_POINT ( 'NONE',  ( 15.40903463028481113, 43.32187500034139305, -47.42413220539094709 ) ) ;
#14001 = DIRECTION ( 'NONE',  ( -1.000000000000000000, 0.000000000000000000, 1.734723475976807094E-17 ) ) ;
#14002 = CARTESIAN_POINT ( 'NONE',  ( -15.45084971874737256, 47.60000000000000142, -47.55282581475767500 ) ) ;
#14003 = CARTESIAN_POINT ( 'NONE',  ( -30.90169943749473802, 28.08125000068280031, 42.53254041760200721 ) ) ;
#14004 = CARTESIAN_POINT ( 'NONE',  ( 15.40903463028482356, 48.52187500034140299, 47.42413220539093999 ) ) ;
#14005 = CARTESIAN_POINT ( 'NONE',  ( 30.81806926056962936, 31.22187500034139873, -42.41743335407647209 ) ) ;
#14006 = CARTESIAN_POINT ( 'NONE',  ( -30.90169943749473447, 28.29999999999999716, 42.53254041760200721 ) ) ;
#14007 = ORIENTED_EDGE ( 'NONE', *, *, #9447, .F. ) ;
#14008 = EDGE_CURVE ( 'NONE', #6897, #13826, #16100, .T. ) ;
#14009 = EDGE_LOOP ( 'NONE', ( #10287, #9853, #7667, #12871 ) ) ;
#14010 = DIRECTION ( 'NONE',  ( -0.3090169943749448977, -0.9510565162951543083, 0.000000000000000000 ) ) ;
#14011 = CARTESIAN_POINT ( 'NONE',  ( 43.87482193696061472, 267.0000000000000000, -10.00000000000000178 ) ) ;
#14012 = FACE_OUTER_BOUND ( 'NONE', #5640, .T. ) ;
#14013 = LINE ( 'NONE', #8704, #9531 ) ;
#14014 = CARTESIAN_POINT ( 'NONE',  ( -49.86468353125000164, 31.85937500034139447, 0.000000000000000000 ) ) ;
#14015 = EDGE_CURVE ( 'NONE', #10751, #12784, #5981, .T. ) ;
#14016 = FILL_AREA_STYLE ('',( #3808 ) ) ;
#14017 = EDGE_CURVE ( 'NONE', #9639, #2321, #16360, .T. ) ;
#14018 = CARTESIAN_POINT ( 'NONE',  ( -3.210462471511496205E-15, 45.42187500034138736, -52.43083105670540789 ) ) ;
#14019 = SURFACE_STYLE_USAGE ( .BOTH. , #8710 ) ;
#14020 = LINE ( 'NONE', #2637, #15759 ) ;
#14021 = AXIS2_PLACEMENT_3D ( 'NONE', #3504, #7328, #9577 ) ;
#14022 = CARTESIAN_POINT ( 'NONE',  ( -49.99999999999999289, 35.88125000068279746, 16.24598481164533226 ) ) ;
#14023 = ADVANCED_FACE ( 'NONE', ( #8245 ), #14705, .F. ) ;
#14024 = LINE ( 'NONE', #8966, #14392 ) ;
#14025 = EDGE_LOOP ( 'NONE', ( #4218, #16015, #7702, #14887, #10796 ) ) ;
#14026 =( BOUNDED_CURVE ( )  B_SPLINE_CURVE ( 2, ( #15761, #14425, #3045, #12021, #5717, #6811, #8118, #16009, #15682, #10788, #8283, #13351, #12104 ),
 .UNSPECIFIED., .F., .F. ) 
 B_SPLINE_CURVE_WITH_KNOTS ( ( 3, 2, 2, 2, 2, 2, 3 ),
 ( 0.6166666666666666963, 0.6199999999999999956, 0.6266666666666667052, 0.6333333333333333037, 0.6400000000000000133, 0.6466666666666666119, 0.6500000000000000222 ),
 .UNSPECIFIED. ) 
 CURVE ( )  GEOMETRIC_REPRESENTATION_ITEM ( )  RATIONAL_B_SPLINE_CURVE ( ( 0.9755282581475768211, 0.9755282581475771542, 1.000000000000000000, 0.9510565162951535312, 1.000000000000000000, 0.9510565162951535312, 1.000000000000000000, 0.9510565162951535312, 1.000000000000000000, 0.9510565162951535312, 1.000000000000000000, 0.9755282581475763770, 0.9755282581475768211 ) ) 
 REPRESENTATION_ITEM ( '' )  );
#14027 = CARTESIAN_POINT ( 'NONE',  ( -15.40903463028480580, 48.32187500034140015, 47.42413220539094709 ) ) ;
#14028 = ORIENTED_EDGE ( 'NONE', *, *, #4907, .T. ) ;
#14029 = CARTESIAN_POINT ( 'NONE',  ( 7.347880794884119933E-15, 52.00000000000000711, 60.00000000000000711 ) ) ;
#14030 = ORIENTED_EDGE ( 'NONE', *, *, #10995, .F. ) ;
#14031 = ORIENTED_EDGE ( 'NONE', *, *, #2024, .F. ) ;
#14032 = ADVANCED_FACE ( 'NONE', ( #7334 ), #4288, .F. ) ;
#14033 = LINE ( 'NONE', #16284, #10027 ) ;
#14034 = FACE_OUTER_BOUND ( 'NONE', #4126, .T. ) ;
#14035 = CARTESIAN_POINT ( 'NONE',  ( -7.919222016226804328, 28.44874571845315003, 50.00000000000000000 ) ) ;
#14036 = CARTESIAN_POINT ( 'NONE',  ( -7.919222016226752814, 37.55125428154683931, -50.00000000000000711 ) ) ;
#14037 = CARTESIAN_POINT ( 'NONE',  ( -2.547328955960238000E-13, 32.28125000068278894, 49.99999999999999289 ) ) ;
#14038 = DIRECTION ( 'NONE',  ( 0.000000000000000000, 1.000000000000000000, 0.000000000000000000 ) ) ;
#14039 = CARTESIAN_POINT ( 'NONE',  ( 7.919222016226809657, 27.22999571913595318, -50.00000000000000000 ) ) ;
#14040 = DIRECTION ( 'NONE',  ( 0.000000000000000000, 1.000000000000000000, 0.000000000000000000 ) ) ;
#14041 = DIRECTION ( 'NONE',  ( 0.000000000000000000, 1.000000000000000000, -0.000000000000000000 ) ) ;
#14042 = CARTESIAN_POINT ( 'NONE',  ( 40.45084971874737079, 38.98125000068279888, -29.38926261462366440 ) ) ;
#14043 = CARTESIAN_POINT ( 'NONE',  ( 45.11452830843730766, 25.00000000000000355, -21.24066852005663719 ) ) ;
#14044 = EDGE_CURVE ( 'NONE', #6639, #6101, #14120, .T. ) ;
#14045 = CARTESIAN_POINT ( 'NONE',  ( 40.45084971874737789, 24.80000000000000426, 29.38926261462365375 ) ) ;
#14046 = CARTESIAN_POINT ( 'NONE',  ( 17.28626291527370284, 40.00000000000000711, -18.64048258526063151 ) ) ;
#14047 = VERTEX_POINT ( 'NONE', #15128 ) ;
#14048 = CARTESIAN_POINT ( 'NONE',  ( 49.86468353125000164, 44.85937500034140157, -6.106662507704105588E-15 ) ) ;
#14049 =( GEOMETRIC_REPRESENTATION_CONTEXT ( 3 ) GLOBAL_UNCERTAINTY_ASSIGNED_CONTEXT ( ( #587 ) ) GLOBAL_UNIT_ASSIGNED_CONTEXT ( ( #11527, #7545, #47 ) ) REPRESENTATION_CONTEXT ( 'NONE', 'WORKASPACE' ) );
#14050 = VERTEX_POINT ( 'NONE', #8735 ) ;
#14051 = EDGE_CURVE ( 'NONE', #9545, #2064, #13802, .T. ) ;
#14052 = DIRECTION ( 'NONE',  ( -0.000000000000000000, -1.000000000000000000, -0.000000000000000000 ) ) ;
#14053 = CARTESIAN_POINT ( 'NONE',  ( 47.28673853953970507, 260.3313524089090265, 10.00000000000000178 ) ) ;
#14054 = CARTESIAN_POINT ( 'NONE',  ( 30.81806926056962936, 27.15937500034139163, -42.41743335407647209 ) ) ;
#14055 = ORIENTED_EDGE ( 'NONE', *, *, #13724, .F. ) ;
#14056 = CARTESIAN_POINT ( 'NONE',  ( 40.45084971874737789, 32.80000000000000426, 29.38926261462365375 ) ) ;
#14057 = CARTESIAN_POINT ( 'NONE',  ( 7.499999999999998224, 25.00000000000000355, 24.29058411375428150 ) ) ;
#14058 = CARTESIAN_POINT ( 'NONE',  ( 47.29342682910159112, 25.00000000000000000, -15.80652463092885007 ) ) ;
#14059 = CARTESIAN_POINT ( 'NONE',  ( -15.40903463028481646, 37.52187500034139589, -47.42413220539093999 ) ) ;
#14060 = CARTESIAN_POINT ( 'NONE',  ( 50.00000000000000000, 30.78125000068279959, -6.123233995736766085E-15 ) ) ;
#14061 = CARTESIAN_POINT ( 'NONE',  ( 49.86468353125000164, 24.85937500034139802, -6.106662507704105588E-15 ) ) ;
#14062 = CARTESIAN_POINT ( 'NONE',  ( 0.000000000000000000, 272.0000000000000000, 89.49773270518483059 ) ) ;
#14063 = CARTESIAN_POINT ( 'NONE',  ( 49.86468353125001585, 30.82187500034139660, 16.20201782572375038 ) ) ;
#14064 = CARTESIAN_POINT ( 'NONE',  ( -2.547328955960238000E-13, 32.50000000000000000, 49.99999999999999289 ) ) ;
#14065 = CARTESIAN_POINT ( 'NONE',  ( 9.657523855033129090E-15, 30.50000000000000000, 52.57311121191334990 ) ) ;
#14066 = CARTESIAN_POINT ( 'NONE',  ( -49.86468353124999453, 29.95937500034139944, 16.20201782572377525 ) ) ;
#14067 = CARTESIAN_POINT ( 'NONE',  ( -40.34137639590981905, 33.72187500034139873, -29.30972558990011478 ) ) ;
#14068 = CARTESIAN_POINT ( 'NONE',  ( -15.45084971874737256, 41.60000000000000142, -47.55282581475767500 ) ) ;
#14069 = ORIENTED_EDGE ( 'NONE', *, *, #3093, .T. ) ;
#14070 = APPLICATION_CONTEXT ( 'automotive_design' ) ;
#14071 = UNCERTAINTY_MEASURE_WITH_UNIT (LENGTH_MEASURE( 1.000000000000000082E-05 ), #10147, 'distance_accuracy_value', 'NONE');
#14072 = CARTESIAN_POINT ( 'NONE',  ( -3.210462471511496205E-15, 37.35937500034140157, -52.43083105670540789 ) ) ;
#14073 = ORIENTED_EDGE ( 'NONE', *, *, #9514, .F. ) ;
#14074 = CARTESIAN_POINT ( 'NONE',  ( 26.23306594128726843, 283.6958662468472880, -4.966131882590523183 ) ) ;
#14075 = CARTESIAN_POINT ( 'NONE',  ( 30.81806926056962936, 49.15937500034138452, -42.41743335407647209 ) ) ;
#14076 = CARTESIAN_POINT ( 'NONE',  ( 3.149380788944009968, 5.278461141749541063, 101.0000000000000000 ) ) ;
#14077 = CARTESIAN_POINT ( 'NONE',  ( -30.81806926056962226, 26.22187500034139518, 42.41743335407647919 ) ) ;
#14078 = DIRECTION ( 'NONE',  ( 0.000000000000000000, 0.000000000000000000, 1.000000000000000000 ) ) ;
#14079 = CARTESIAN_POINT ( 'NONE',  ( -49.86468353124999453, 40.02187500034140299, 16.20201782572377525 ) ) ;
#14080 = CARTESIAN_POINT ( 'NONE',  ( -3.210462471511496205E-15, 41.35937500034138736, -52.43083105670540789 ) ) ;
#14081 = CARTESIAN_POINT ( 'NONE',  ( -50.00000000000000000, 48.00000000000000000, 0.000000000000000000 ) ) ;
#14082 = PRODUCT_DEFINITION_SHAPE ( 'NONE', 'NONE',  #16466 ) ;
#14083 = CARTESIAN_POINT ( 'NONE',  ( -15.45084971874737256, 25.38125000068279746, -47.55282581475767500 ) ) ;
#14084 = CARTESIAN_POINT ( 'NONE',  ( 16.92534237191551938, 26.98475202694456598, 93.72602301361716570 ) ) ;
#14085 = CARTESIAN_POINT ( 'NONE',  ( 40.34137639590981905, 30.72187500034139518, 29.30972558990010768 ) ) ;
#14086 = EDGE_CURVE ( 'NONE', #1062, #14577, #10153, .T. ) ;
#14087 = FACE_OUTER_BOUND ( 'NONE', #3137, .T. ) ;
#14088 = ORIENTED_EDGE ( 'NONE', *, *, #11387, .F. ) ;
#14089 = CARTESIAN_POINT ( 'NONE',  ( -49.99999999999999289, 37.88125000068279746, 16.24598481164533226 ) ) ;
#14090 = ORIENTED_EDGE ( 'NONE', *, *, #8648, .F. ) ;
#14091 = DIRECTION ( 'NONE',  ( -2.312964634635742464E-16, -0.000000000000000000, 1.000000000000000000 ) ) ;
#14092 = FACE_OUTER_BOUND ( 'NONE', #8236, .T. ) ;
#14093 = FACE_OUTER_BOUND ( 'NONE', #6819, .T. ) ;
#14094 = CARTESIAN_POINT ( 'NONE',  ( -15.40903463028480580, 48.32187500034140015, 47.42413220539094709 ) ) ;
#14095 = ADVANCED_FACE ( 'NONE', ( #13720 ), #13878, .T. ) ;
#14096 = CARTESIAN_POINT ( 'NONE',  ( -15.40903463028480580, 32.25937500034140015, 47.42413220539094709 ) ) ;
#14097 = CARTESIAN_POINT ( 'NONE',  ( -10.69075041230567891, 8.636095224584611429, 102.0000000000000142 ) ) ;
#14098 = CARTESIAN_POINT ( 'NONE',  ( 49.86468353125000164, 44.92187500034140157, -6.106662507704105588E-15 ) ) ;
#14099 = SHAPE_DEFINITION_REPRESENTATION ( #1749, #6178 ) ;
#14100 = CARTESIAN_POINT ( 'NONE',  ( 2.499999999999999556, 247.0000000000000568, -49.17157287525380127 ) ) ;
#14101 = DIRECTION ( 'NONE',  ( -0.000000000000000000, -1.000000000000000000, -0.000000000000000000 ) ) ;
#14102 = CARTESIAN_POINT ( 'NONE',  ( 0.000000000000000000, 50.00000000000000000, 0.000000000000000000 ) ) ;
#14103 = ORIENTED_EDGE ( 'NONE', *, *, #3363, .T. ) ;
#14104 = CARTESIAN_POINT ( 'NONE',  ( -49.86468353124999453, 48.02187500034139589, 16.20201782572377525 ) ) ;
#14105 = ORIENTED_EDGE ( 'NONE', *, *, #12611, .F. ) ;
#14106 = CARTESIAN_POINT ( 'NONE',  ( -40.45084971874737079, 26.20000000000000284, 29.38926261462367151 ) ) ;
#14107 = EDGE_CURVE ( 'NONE', #4375, #10042, #2413, .T. ) ;
#14108 = VERTEX_POINT ( 'NONE', #3755 ) ;
#14109 = ORIENTED_EDGE ( 'NONE', *, *, #9057, .F. ) ;
#14110 = CARTESIAN_POINT ( 'NONE',  ( 14.43699227201001101, 100.7369268407877598, -5.000000000000000000 ) ) ;
#14111 = CARTESIAN_POINT ( 'NONE',  ( -49.86468353125000164, 49.89062500034140157, 0.000000000000000000 ) ) ;
#14112 = CARTESIAN_POINT ( 'NONE',  ( 8.446640517145639571E-15, 28.49999999999999645, 50.00000000000000000 ) ) ;
#14113 = CARTESIAN_POINT ( 'NONE',  ( -30.90169943749474868, 25.69999999999999929, -42.53254041760200721 ) ) ;
#14114 = DIRECTION ( 'NONE',  ( 0.1045284632676435066, 0.9945218953682744001, 0.000000000000000000 ) ) ;
#14115 = DIRECTION ( 'NONE',  ( 1.000000000000000000, 1.962715704248044508E-14, 0.000000000000000000 ) ) ;
#14116 = CARTESIAN_POINT ( 'NONE',  ( 0.000000000000000000, 267.0000000000000000, 0.000000000000000000 ) ) ;
#14117 = DIRECTION ( 'NONE',  ( 0.1045284632676570929, -0.9945218953682730678, 0.000000000000000000 ) ) ;
#14118 = FACE_OUTER_BOUND ( 'NONE', #7156, .T. ) ;
#14119 = CARTESIAN_POINT ( 'NONE',  ( -30.90169943749474868, 43.48125000068279178, -42.53254041760200721 ) ) ;
#14120 =( BOUNDED_CURVE ( )  B_SPLINE_CURVE ( 2, ( #7658, #7599, #4854, #998, #9911, #7337, #12487, #3679, #8900, #6171, #1080, #11168, #7571 ),
 .UNSPECIFIED., .F., .F. ) 
 B_SPLINE_CURVE_WITH_KNOTS ( ( 3, 2, 2, 2, 2, 2, 3 ),
 ( 0.7833333333333333259, 0.7866666666666666252, 0.7933333333333333348, 0.8000000000000000444, 0.8066666666666666430, 0.8133333333333333526, 0.8166666666666666519 ),
 .UNSPECIFIED. ) 
 CURVE ( )  GEOMETRIC_REPRESENTATION_ITEM ( )  RATIONAL_B_SPLINE_CURVE ( ( 0.9755282581475768211, 0.9755282581475768211, 1.000000000000000000, 0.9510565162951535312, 1.000000000000000000, 0.9510565162951535312, 1.000000000000000000, 0.9510565162951535312, 1.000000000000000000, 0.9510565162951535312, 1.000000000000000000, 0.9755282581475768211, 0.9755282581475768211 ) ) 
 REPRESENTATION_ITEM ( '' )  );
#14121 = CARTESIAN_POINT ( 'NONE',  ( -30.27664397204038593, 40.00000000000000711, 26.14048258526057467 ) ) ;
#14122 = EDGE_CURVE ( 'NONE', #3157, #9937, #696, .T. ) ;
#14123 = CARTESIAN_POINT ( 'NONE',  ( 40.45084971874737079, 25.19999999999999929, -29.38926261462366440 ) ) ;
#14124 = LINE ( 'NONE', #4252, #5921 ) ;
#14125 = ORIENTED_EDGE ( 'NONE', *, *, #16428, .T. ) ;
#14126 = CARTESIAN_POINT ( 'NONE',  ( 15.40903463028482356, 40.45937500034139589, 47.42413220539093999 ) ) ;
#14127 = EDGE_CURVE ( 'NONE', #8525, #10911, #11476, .T. ) ;
#14128 = ORIENTED_EDGE ( 'NONE', *, *, #2183, .F. ) ;
#14129 = FILL_AREA_STYLE_COLOUR ( '', #6795 ) ;
#14130 = CARTESIAN_POINT ( 'NONE',  ( 43.87482193696061472, 257.0000000000001137, -10.00000000000000000 ) ) ;
#14131 = CARTESIAN_POINT ( 'NONE',  ( -49.86468353125000164, 29.85937500034139802, 0.000000000000000000 ) ) ;
#14132 = ORIENTED_EDGE ( 'NONE', *, *, #6844, .T. ) ;
#14133 = EDGE_CURVE ( 'NONE', #16188, #14909, #14292, .T. ) ;
#14134 = B_SPLINE_CURVE_WITH_KNOTS ( 'NONE', 3,
 ( #1836, #15646, #3008, #4350 ),
 .UNSPECIFIED., .F., .F.,
 ( 4, 4 ),
 ( 2.829004760677457000E-07, 0.001414802801989367004 ),
 .UNSPECIFIED. ) ;
#14135 = CARTESIAN_POINT ( 'NONE',  ( 49.99999999999999289, 27.10000000000000142, -16.24598481164532160 ) ) ;
#14136 = PLANE ( 'NONE',  #2267 ) ;
#14137 = LINE ( 'NONE', #4263, #13872 ) ;
#14138 = CARTESIAN_POINT ( 'NONE',  ( 15.40903463028481113, 35.32187500034139305, -47.42413220539094709 ) ) ;
#14139 = DIRECTION ( 'NONE',  ( 0.4067366430758010964, -0.9135454576426004225, 0.000000000000000000 ) ) ;
#14140 = CARTESIAN_POINT ( 'NONE',  ( -49.86468353124999453, 21.95937500034139234, 16.20201782572377169 ) ) ;
#14141 = PLANE ( 'NONE',  #1230 ) ;
#14142 = CARTESIAN_POINT ( 'NONE',  ( 40.34137639590981905, 30.72187500034139518, 29.30972558990010768 ) ) ;
#14143 = CARTESIAN_POINT ( 'NONE',  ( -0.5000000000000000000, 245.0000000000000284, -49.99999999999999289 ) ) ;
#14144 = MANIFOLD_SOLID_BREP ( 'Cut-Extrude1', #4698 ) ;
#14145 = CARTESIAN_POINT ( 'NONE',  ( -49.99999999999999289, 28.10000000000000497, 16.24598481164533226 ) ) ;
#14146 = CARTESIAN_POINT ( 'NONE',  ( -15.40903463028480580, 34.25937500034139305, 47.42413220539094709 ) ) ;
#14147 = CARTESIAN_POINT ( 'NONE',  ( -49.86468353124999453, 30.02187500034139234, 16.20201782572377525 ) ) ;
#14148 = VECTOR ( 'NONE', #13735, 1000.000000000000000 ) ;
#14149 = ORIENTED_EDGE ( 'NONE', *, *, #5214, .T. ) ;
#14150 = CARTESIAN_POINT ( 'NONE',  ( -15.40903463028480580, 38.25937500034140015, 47.42413220539094709 ) ) ;
#14151 = VERTEX_POINT ( 'NONE', #6756 ) ;
#14152 = ORIENTED_EDGE ( 'NONE', *, *, #4345, .F. ) ;
#14153 = EDGE_CURVE ( 'NONE', #10059, #3819, #10416, .T. ) ;
#14154 = CARTESIAN_POINT ( 'NONE',  ( 27.40717431545391491, 282.1599167565164521, -11.20358715772642810 ) ) ;
#14155 = CARTESIAN_POINT ( 'NONE',  ( 49.99999999999999289, 20.88125000068279746, -16.24598481164532160 ) ) ;
#14156 = EDGE_CURVE ( 'NONE', #3758, #13942, #14493, .T. ) ;
#14157 = CARTESIAN_POINT ( 'NONE',  ( 0.000000000000000000, 50.00000000000000000, 0.000000000000000000 ) ) ;
#14158 = CARTESIAN_POINT ( 'NONE',  ( 49.86468353125000164, 24.92187500034139802, -6.106662507704105588E-15 ) ) ;
#14159 = CONICAL_SURFACE ( 'NONE', #8581, 100.0000000000000000, 0.1745329251994333364 ) ;
#14160 = LINE ( 'NONE', #12515, #4143 ) ;
#14161 = CARTESIAN_POINT ( 'NONE',  ( -15.40903463028480580, 36.32187500034140015, 47.42413220539094709 ) ) ;
#14162 = CARTESIAN_POINT ( 'NONE',  ( 15.40903463028481113, 39.25937500034140015, -47.42413220539094709 ) ) ;
#14163 = DIRECTION ( 'NONE',  ( -0.000000000000000000, 1.000000000000000000, -0.000000000000000000 ) ) ;
#14164 = CARTESIAN_POINT ( 'NONE',  ( -15.45084971874736368, 48.40000000000000568, 47.55282581475768211 ) ) ;
#14165 = CARTESIAN_POINT ( 'NONE',  ( -40.45084971874737079, 19.98125000068279888, 29.38926261462367151 ) ) ;
#14166 = CARTESIAN_POINT ( 'NONE',  ( 16.59466974644969994, 28.08544099924165494, 93.58803292011415920 ) ) ;
#14167 = CARTESIAN_POINT ( 'NONE',  ( 30.81806926056964002, 28.62187500034140086, 42.41743335407647209 ) ) ;
#14168 = CARTESIAN_POINT ( 'NONE',  ( 8.446640517145639571E-15, 28.49999999999999645, 50.00000000000000000 ) ) ;
#14169 = VERTEX_POINT ( 'NONE', #10479 ) ;
#14170 = CARTESIAN_POINT ( 'NONE',  ( 9.657523855033129090E-15, 40.28125000068278894, 52.57311121191334990 ) ) ;
#14171 = VERTEX_POINT ( 'NONE', #15539 ) ;
#14172 = CARTESIAN_POINT ( 'NONE',  ( 15.45084971874736723, 49.18125000068279462, -47.55282581475768211 ) ) ;
#14173 = DIRECTION ( 'NONE',  ( -6.938893903907231459E-18, 1.000000000000000000, 5.551115123125782702E-17 ) ) ;
#14174 = EDGE_CURVE ( 'NONE', #7011, #13297, #242, .T. ) ;
#14175 = DIRECTION ( 'NONE',  ( 0.9361168066628590134, -0.08189960831908912886, 0.3420201433256691570 ) ) ;
#14176 = CARTESIAN_POINT ( 'NONE',  ( -15.40903463028481646, 47.52187500034139589, -47.42413220539093999 ) ) ;
#14177 = EDGE_CURVE ( 'NONE', #14691, #14171, #7981, .T. ) ;
#14178 = CARTESIAN_POINT ( 'NONE',  ( -15.40903463028481646, 27.45937500034139944, -47.42413220539093999 ) ) ;
#14179 = DIRECTION ( 'NONE',  ( 0.000000000000000000, 0.000000000000000000, -1.000000000000000000 ) ) ;
#14180 = VECTOR ( 'NONE', #6786, 1000.000000000000114 ) ;
#14181 = CARTESIAN_POINT ( 'NONE',  ( 49.86468353124999453, 45.02187500034138878, -16.20201782572376104 ) ) ;
#14182 = CARTESIAN_POINT ( 'NONE',  ( 0.000000000000000000, 0.000000000000000000, 0.000000000000000000 ) ) ;
#14183 = FACE_OUTER_BOUND ( 'NONE', #9460, .T. ) ;
#14184 = CARTESIAN_POINT ( 'NONE',  ( 49.86468353125000164, 46.92187500034139447, -6.106662507704105588E-15 ) ) ;
#14185 = CARTESIAN_POINT ( 'NONE',  ( 19.99999999999999289, 307.0000000000000568, 2.500000000000002220 ) ) ;
#14186 = VERTEX_POINT ( 'NONE', #14046 ) ;
#14187 = CARTESIAN_POINT ( 'NONE',  ( 15.40903463028481113, 21.25937500034139660, -47.42413220539094709 ) ) ;
#14188 = VERTEX_POINT ( 'NONE', #14205 ) ;
#14189 = CARTESIAN_POINT ( 'NONE',  ( -48.98979485566356828, 261.9999999999999432, -9.999999999999994671 ) ) ;
#14190 = ORIENTED_EDGE ( 'NONE', *, *, #10992, .F. ) ;
#14191 = ORIENTED_EDGE ( 'NONE', *, *, #6967, .T. ) ;
#14192 = VECTOR ( 'NONE', #14888, 1000.000000000000000 ) ;
#14193 = FACE_OUTER_BOUND ( 'NONE', #9248, .T. ) ;
#14194 = CARTESIAN_POINT ( 'NONE',  ( 40.45084971874737789, 38.58125000068280031, 29.38926261462365375 ) ) ;
#14195 = CARTESIAN_POINT ( 'NONE',  ( -50.00000000000000000, 28.00000000000000000, 0.000000000000000000 ) ) ;
#14196 = CARTESIAN_POINT ( 'NONE',  ( 40.45084971874737079, 23.20000000000000284, -29.38926261462366440 ) ) ;
#14197 = CARTESIAN_POINT ( 'NONE',  ( -49.86468353124999453, 47.95937500034138878, 16.20201782572377525 ) ) ;
#14198 = FACE_OUTER_BOUND ( 'NONE', #3072, .T. ) ;
#14199 = FACE_BOUND ( 'NONE', #2523, .T. ) ;
#14200 = CARTESIAN_POINT ( 'NONE',  ( -49.86468353125000164, 21.92187500034139802, 0.000000000000000000 ) ) ;
#14201 = CARTESIAN_POINT ( 'NONE',  ( -13.33959974903384627, 33.83821319854129683, 101.0000000000000000 ) ) ;
#14202 = CARTESIAN_POINT ( 'NONE',  ( -30.90169943749474868, 37.48125000068279888, -42.53254041760200721 ) ) ;
#14203 = DIRECTION ( 'NONE',  ( 0.000000000000000000, 0.000000000000000000, 1.000000000000000000 ) ) ;
#14204 = CARTESIAN_POINT ( 'NONE',  ( 50.00000000000000000, 20.78125000068279959, -6.123233995736766085E-15 ) ) ;
#14205 = CARTESIAN_POINT ( 'NONE',  ( -5.000000000000000000, 99.58041009241402719, -7.580410092413988998 ) ) ;
#14206 = ORIENTED_EDGE ( 'NONE', *, *, #3362, .F. ) ;
#14207 = CARTESIAN_POINT ( 'NONE',  ( 30.81806926056964002, 38.55937500034140442, 42.41743335407647209 ) ) ;
#14208 = ORIENTED_EDGE ( 'NONE', *, *, #6165, .F. ) ;
#14209 = CARTESIAN_POINT ( 'NONE',  ( 7.919222016226809657, 43.44874571845315359, -50.00000000000000000 ) ) ;
#14210 = AXIS2_PLACEMENT_3D ( 'NONE', #15099, #3726, #8785 ) ;
#14211 = DIRECTION ( 'NONE',  ( -0.3090169943749573878, 0.9510565162951503115, 0.000000000000000000 ) ) ;
#14212 = CARTESIAN_POINT ( 'NONE',  ( -49.86468353124999453, 23.95937500034138878, 16.20201782572377525 ) ) ;
#14213 = ADVANCED_FACE ( 'NONE', ( #9071 ), #5508, .T. ) ;
#14214 = VERTEX_POINT ( 'NONE', #12977 ) ;
#14215 = PLANE ( 'NONE',  #4417 ) ;
#14216 = CARTESIAN_POINT ( 'NONE',  ( -10.68402110179033926, 36.37206659422378863, 92.97581280613414378 ) ) ;
#14217 = DIRECTION ( 'NONE',  ( -1.000000000000000000, 0.000000000000000000, 0.000000000000000000 ) ) ;
#14218 = CARTESIAN_POINT ( 'NONE',  ( 30.81806926056964002, 26.62187500034139731, 42.41743335407646498 ) ) ;
#14219 =( BOUNDED_CURVE ( )  B_SPLINE_CURVE ( 3, ( #11468, #1149, #15120, #8979 ),
 .UNSPECIFIED., .F., .F. ) 
 B_SPLINE_CURVE_WITH_KNOTS ( ( 4, 4 ),
 ( 0.000000000000000000, 1.570796326794896780 ),
 .UNSPECIFIED. ) 
 CURVE ( )  GEOMETRIC_REPRESENTATION_ITEM ( )  RATIONAL_B_SPLINE_CURVE ( ( 1.000000000000000000, 0.8047378541243649375, 0.8047378541243649375, 1.000000000000000000 ) ) 
 REPRESENTATION_ITEM ( '' )  );
#14220 = CARTESIAN_POINT ( 'NONE',  ( -50.00000000000000000, 29.78125000068279959, 0.000000000000000000 ) ) ;
#14221 = DIRECTION ( 'NONE',  ( -1.000000000000000000, 0.000000000000000000, 0.000000000000000000 ) ) ;
#14222 = CARTESIAN_POINT ( 'NONE',  ( -48.20095974065431932, 20.00000000000001066, 12.77318064350212623 ) ) ;
#14223 = CARTESIAN_POINT ( 'NONE',  ( -49.86468353124999453, 30.02187500034139234, 16.20201782572377169 ) ) ;
#14224 = EDGE_CURVE ( 'NONE', #8209, #5006, #14124, .T. ) ;
#14225 = DIRECTION ( 'NONE',  ( 0.000000000000000000, -0.000000000000000000, 1.000000000000000000 ) ) ;
#14226 = AXIS2_PLACEMENT_3D ( 'NONE', #5252, #15518, #2898 ) ;
#14227 = CARTESIAN_POINT ( 'NONE',  ( -15.45084971874736368, 28.40000000000000213, 47.55282581475768211 ) ) ;
#14228 = CARTESIAN_POINT ( 'NONE',  ( 49.86468353125001585, 30.75937500034139305, 16.20201782572375038 ) ) ;
#14229 = CIRCLE ( 'NONE', #953, 14.08089297201391155 ) ;
#14230 = CARTESIAN_POINT ( 'NONE',  ( 15.40903463028481113, 27.32187500034139660, -47.42413220539094709 ) ) ;
#14231 = AXIS2_PLACEMENT_3D ( 'NONE', #8334, #14091, #2790 ) ;
#14232 = AXIS2_PLACEMENT_3D ( 'NONE', #8806, #6407, #15280 ) ;
#14233 = DIRECTION ( 'NONE',  ( 0.9781476007338069101, -0.2079116908177532363, 0.000000000000000000 ) ) ;
#14234 = EDGE_CURVE ( 'NONE', #15357, #436, #12803, .T. ) ;
#14235 = ORIENTED_EDGE ( 'NONE', *, *, #14334, .F. ) ;
#14236 = PRODUCT_DEFINITION_CONTEXT ( 'detailed design', #14070, 'design' ) ;
#14237 = CARTESIAN_POINT ( 'NONE',  ( 49.86468353125000164, 32.85937500034139447, -6.106662507704105588E-15 ) ) ;
#14238 = ORIENTED_EDGE ( 'NONE', *, *, #9780, .T. ) ;
#14239 = CARTESIAN_POINT ( 'NONE',  ( 22.46613188258983485, 283.6958662468469470, -8.733065941287611267 ) ) ;
#14240 = CARTESIAN_POINT ( 'NONE',  ( -49.86468353124999453, 49.75937500034138594, -16.20201782572375393 ) ) ;
#14241 = ADVANCED_FACE ( 'NONE', ( #1737 ), #9319, .F. ) ;
#14242 = AXIS2_PLACEMENT_3D ( 'NONE', #10337, #8832, #4018 ) ;
#14243 = AXIS2_PLACEMENT_3D ( 'NONE', #11573, #3771, #11260 ) ;
#14244 = CARTESIAN_POINT ( 'NONE',  ( 9.877534094663406705, 8.054089844915898411, 101.0000000000000000 ) ) ;
#14245 = AXIS2_PLACEMENT_3D ( 'NONE', #1889, #8142, #13124 ) ;
#14246 = CARTESIAN_POINT ( 'NONE',  ( 26.95005104082769520, 283.0244618719127629, 6.400102081653809449 ) ) ;
#14247 = DIRECTION ( 'NONE',  ( 0.000000000000000000, 0.000000000000000000, 1.000000000000000000 ) ) ;
#14248 = CARTESIAN_POINT ( 'NONE',  ( -40.34137639590981905, 33.72187500034139873, -29.30972558990011478 ) ) ;
#14249 = CARTESIAN_POINT ( 'NONE',  ( 40.34137639590981195, 43.05937500034139731, -29.30972558990011834 ) ) ;
#14250 = DIRECTION ( 'NONE',  ( 0.000000000000000000, 0.7071067811865487940, -0.7071067811865463515 ) ) ;
#14251 = CARTESIAN_POINT ( 'NONE',  ( -49.99999999999999289, 40.09999999999999432, 16.24598481164533226 ) ) ;
#14252 = CARTESIAN_POINT ( 'NONE',  ( -50.00000000000000000, 19.78125000068279604, 0.000000000000000000 ) ) ;
#14253 = CARTESIAN_POINT ( 'NONE',  ( -3.210462471511496205E-15, 45.42187500034139447, -52.43083105670540789 ) ) ;
#14254 = CARTESIAN_POINT ( 'NONE',  ( -15.40903463028480580, 26.32187500034140015, 47.42413220539094709 ) ) ;
#14255 = CIRCLE ( 'NONE', #7105, 50.00000000000000000 ) ;
#14256 = CARTESIAN_POINT ( 'NONE',  ( 16.68146630878714731, 20.24395310072318921, 101.6666710451724214 ) ) ;
#14257 = ORIENTED_EDGE ( 'NONE', *, *, #13422, .F. ) ;
#14258 = CARTESIAN_POINT ( 'NONE',  ( 15.45084971874736723, 35.18125000068280173, -47.55282581475768211 ) ) ;
#14259 = ORIENTED_EDGE ( 'NONE', *, *, #9388, .T. ) ;
#14260 = CARTESIAN_POINT ( 'NONE',  ( 8.446640517145639571E-15, 48.28125000068279604, 50.00000000000000000 ) ) ;
#14261 = CARTESIAN_POINT ( 'NONE',  ( 14.53285685708578256, 14.68680145065703080, 102.0000000000000142 ) ) ;
#14262 = CARTESIAN_POINT ( 'NONE',  ( 0.000000000000000000, 273.6527036446661896, 0.000000000000000000 ) ) ;
#14263 = CARTESIAN_POINT ( 'NONE',  ( 40.34137639590981905, 46.72187500034139873, 29.30972558990010768 ) ) ;
#14264 = CARTESIAN_POINT ( 'NONE',  ( 9.631387414534489405E-15, 24.35937500034139802, 52.43083105670540789 ) ) ;
#14265 = DIRECTION ( 'NONE',  ( -0.000000000000000000, 1.000000000000000000, -0.000000000000000000 ) ) ;
#14266 = CARTESIAN_POINT ( 'NONE',  ( 40.34137639590981905, 42.72187500034139873, 29.30972558990010768 ) ) ;
#14267 = DIRECTION ( 'NONE',  ( 1.000000000000000000, 0.000000000000000000, 0.000000000000000000 ) ) ;
#14268 = CARTESIAN_POINT ( 'NONE',  ( 5.510910596163089556E-15, 267.0000000000000000, -45.00000000000000000 ) ) ;
#14269 = CARTESIAN_POINT ( 'NONE',  ( -30.81806926056962226, 46.22187500034139163, 42.41743335407647919 ) ) ;
#14270 = DIRECTION ( 'NONE',  ( 0.5000000000000039968, -0.8660254037844363761, 0.000000000000000000 ) ) ;
#14271 = VERTEX_POINT ( 'NONE', #2990 ) ;
#14272 = CARTESIAN_POINT ( 'NONE',  ( -15.40903463028481646, 45.52187500034139589, -47.42413220539093999 ) ) ;
#14273 = VECTOR ( 'NONE', #3142, 1000.000000000000000 ) ;
#14274 = ADVANCED_FACE ( 'NONE', ( #8058 ), #6498, .F. ) ;
#14275 = ORIENTED_EDGE ( 'NONE', *, *, #11887, .T. ) ;
#14276 = DIRECTION ( 'NONE',  ( 0.000000000000000000, 0.000000000000000000, -1.000000000000000000 ) ) ;
#14277 = ORIENTED_EDGE ( 'NONE', *, *, #8336, .T. ) ;
#14278 = EDGE_LOOP ( 'NONE', ( #5720, #565, #11889, #1739, #670, #6970, #2608, #8680, #8388, #3778, #1588, #13662, #13392, #12898, #14907, #15271, #4444, #11369, #775, #16206, #14190, #23, #13698, #5786, #5482, #15683, #14412, #13483, #3365 ) ) ;
#14279 = CARTESIAN_POINT ( 'NONE',  ( -15.45084971874737256, 43.38125000068279746, -47.55282581475767500 ) ) ;
#14280 = CARTESIAN_POINT ( 'NONE',  ( -0.5000000000000000000, 242.0000000000000284, 49.99999999999999289 ) ) ;
#14281 = FACE_OUTER_BOUND ( 'NONE', #12813, .T. ) ;
#14282 = CARTESIAN_POINT ( 'NONE',  ( -30.90169943749474868, 23.69999999999999929, -42.53254041760200721 ) ) ;
#14283 = CARTESIAN_POINT ( 'NONE',  ( 30.81806926056964002, 42.55937500034139020, 42.41743335407647209 ) ) ;
#14284 = CARTESIAN_POINT ( 'NONE',  ( 40.45084971874737079, 48.98125000068279888, -29.38926261462366440 ) ) ;
#14285 = DIRECTION ( 'NONE',  ( -0.000000000000000000, -0.000000000000000000, 1.000000000000000000 ) ) ;
#14286 = CARTESIAN_POINT ( 'NONE',  ( 2.600676159226420495E-13, 33.28125000068279604, -49.99999999999999289 ) ) ;
#14287 = VECTOR ( 'NONE', #13628, 1000.000000000000000 ) ;
#14288 = FACE_BOUND ( 'NONE', #13100, .T. ) ;
#14289 = CARTESIAN_POINT ( 'NONE',  ( -30.90169943749473802, 42.08125000068279320, 42.53254041760200721 ) ) ;
#14290 = CARTESIAN_POINT ( 'NONE',  ( -50.00000000000000000, 37.78125000068280315, 0.000000000000000000 ) ) ;
#14291 = CARTESIAN_POINT ( 'NONE',  ( 15.45084971874737789, 22.38125000068280102, 47.55282581475767500 ) ) ;
#14292 = LINE ( 'NONE', #74, #9214 ) ;
#14293 = ORIENTED_EDGE ( 'NONE', *, *, #15309, .F. ) ;
#14294 = CARTESIAN_POINT ( 'NONE',  ( 15.40903463028482356, 36.45937500034139589, 47.42413220539093999 ) ) ;
#14295 = ORIENTED_EDGE ( 'NONE', *, *, #11199, .F. ) ;
#14296 = VERTEX_POINT ( 'NONE', #486 ) ;
#14297 = CARTESIAN_POINT ( 'NONE',  ( 30.90169943749474157, 47.08125000068280031, -42.53254041760200721 ) ) ;
#14298 = VECTOR ( 'NONE', #3060, 1000.000000000000000 ) ;
#14299 = FACE_OUTER_BOUND ( 'NONE', #8471, .T. ) ;
#14300 = CARTESIAN_POINT ( 'NONE',  ( 40.34137639590981195, 21.05937500034139376, -29.30972558990011834 ) ) ;
#14301 = EDGE_LOOP ( 'NONE', ( #12854, #875, #14109, #2540 ) ) ;
#14302 = DIRECTION ( 'NONE',  ( 0.000000000000000000, 0.000000000000000000, 1.000000000000000000 ) ) ;
#14303 = CARTESIAN_POINT ( 'NONE',  ( -2.547328955960238000E-13, 34.50000000000000000, 49.99999999999999289 ) ) ;
#14304 = DIRECTION ( 'NONE',  ( -0.5877852522924797984, 0.8090169943749424553, 0.000000000000000000 ) ) ;
#14305 = CARTESIAN_POINT ( 'NONE',  ( 49.86468353124999453, 31.02187500034139589, -16.20201782572376104 ) ) ;
#14306 = EDGE_CURVE ( 'NONE', #1328, #4312, #12554, .T. ) ;
#14307 = CARTESIAN_POINT ( 'NONE',  ( -2.547328955960238000E-13, 30.28125000068279604, 49.99999999999999289 ) ) ;
#14308 = EDGE_CURVE ( 'NONE', #2312, #10814, #14529, .T. ) ;
#14309 = CARTESIAN_POINT ( 'NONE',  ( 2.500000000000000000, 242.0000000000000284, 47.99999999999999289 ) ) ;
#14310 = CARTESIAN_POINT ( 'NONE',  ( -46.44184698740843231, 20.00000000000000355, 18.15679736478566753 ) ) ;
#14311 = CARTESIAN_POINT ( 'NONE',  ( -15.40903463028481646, 29.52187500034139589, -47.42413220539093999 ) ) ;
#14312 = CARTESIAN_POINT ( 'NONE',  ( 7.580410092413998768, 101.3368000520362813, -5.000000000000000000 ) ) ;
#14313 = AXIS2_PLACEMENT_3D ( 'NONE', #9387, #14437, #9628 ) ;
#14314 = CARTESIAN_POINT ( 'NONE',  ( -40.45084971874737079, 34.20000000000000284, 29.38926261462367151 ) ) ;
#14315 = CARTESIAN_POINT ( 'NONE',  ( 15.40903463028482356, 32.45937500034138878, 47.42413220539093999 ) ) ;
#14316 = FACE_OUTER_BOUND ( 'NONE', #5228, .T. ) ;
#14317 = VERTEX_POINT ( 'NONE', #4329 ) ;
#14318 = CARTESIAN_POINT ( 'NONE',  ( -49.86468353125000164, 27.85937500034139447, 0.000000000000000000 ) ) ;
#14319 = VERTEX_POINT ( 'NONE', #16028 ) ;
#14320 = ADVANCED_FACE ( 'NONE', ( #9633 ), #8470, .F. ) ;
#14321 = PLANE ( 'NONE',  #12655 ) ;
#14323 =( BOUNDED_CURVE ( )  B_SPLINE_CURVE ( 2, ( #2696, #12844, #4454, #4365, #9519, #8263, #10436, #10682, #14566, #9430, #14480, #3113, #7022 ),
 .UNSPECIFIED., .F., .F. ) 
 B_SPLINE_CURVE_WITH_KNOTS ( ( 3, 2, 2, 2, 2, 2, 3 ),
 ( 0.1833333333333333481, 0.1866666666666666752, 0.1933333333333333293, 0.2000000000000000111, 0.2066666666666666652, 0.2133333333333333470, 0.2166666666666666741 ),
 .UNSPECIFIED. ) 
 CURVE ( )  GEOMETRIC_REPRESENTATION_ITEM ( )  RATIONAL_B_SPLINE_CURVE ( ( 0.9755282581475767101, 0.9755282581475768211, 1.000000000000000000, 0.9510565162951535312, 1.000000000000000000, 0.9510565162951535312, 1.000000000000000000, 0.9510565162951535312, 1.000000000000000000, 0.9510565162951535312, 1.000000000000000000, 0.9755282581475768211, 0.9755282581475768211 ) ) 
 REPRESENTATION_ITEM ( '' )  );
#14322 = CARTESIAN_POINT ( 'NONE',  ( -3.210462471511496205E-15, 41.35937500034138736, -52.43083105670540789 ) ) ;
#14324 =( GEOMETRIC_REPRESENTATION_CONTEXT ( 3 ) GLOBAL_UNCERTAINTY_ASSIGNED_CONTEXT ( ( #15405 ) ) GLOBAL_UNIT_ASSIGNED_CONTEXT ( ( #2571, #8888, #1234 ) ) REPRESENTATION_CONTEXT ( 'NONE', 'WORKASPACE' ) );
#14325 = FACE_OUTER_BOUND ( 'NONE', #15094, .T. ) ;
#14326 = CARTESIAN_POINT ( 'NONE',  ( 40.34137639590981905, 20.72187500034139873, 29.30972558990010768 ) ) ;
#14327 = CARTESIAN_POINT ( 'NONE',  ( -24.76951992798375102, 286.3033656649002410, 7.269519927983750129 ) ) ;
#14328 = CARTESIAN_POINT ( 'NONE',  ( 30.81806926056964002, 38.62187500034139731, 42.41743335407647209 ) ) ;
#14329 = CARTESIAN_POINT ( 'NONE',  ( 30.81806926056964002, 36.55937500034139731, 42.41743335407646498 ) ) ;
#14330 = PLANE ( 'NONE',  #12364 ) ;
#14331 = CARTESIAN_POINT ( 'NONE',  ( -30.90169943749474868, 43.70000000000000284, -42.53254041760200721 ) ) ;
#14332 = CARTESIAN_POINT ( 'NONE',  ( 40.45084971874737789, 20.58125000068280031, 29.38926261462365375 ) ) ;
#14333 = CARTESIAN_POINT ( 'NONE',  ( -30.81806926056962226, 44.22187500034139163, 42.41743335407647919 ) ) ;
#14334 = EDGE_CURVE ( 'NONE', #6698, #11113, #9396, .T. ) ;
#14335 = CARTESIAN_POINT ( 'NONE',  ( -40.34137639590981905, 29.72187500034139518, -29.30972558990011478 ) ) ;
#14336 = CARTESIAN_POINT ( 'NONE',  ( 40.34137639590981905, 46.65937500034139873, 29.30972558990010768 ) ) ;
#14337 = ORIENTED_EDGE ( 'NONE', *, *, #11252, .F. ) ;
#14338 = CARTESIAN_POINT ( 'NONE',  ( -15.45084971874736368, 28.18125000068279817, 47.55282581475768211 ) ) ;
#14339 = EDGE_CURVE ( 'NONE', #10702, #7079, #813, .T. ) ;
#14340 = ORIENTED_EDGE ( 'NONE', *, *, #14224, .F. ) ;
#14341 = CARTESIAN_POINT ( 'NONE',  ( 7.499999999999998224, 40.00000000000000711, 24.29058411375428150 ) ) ;
#14342 = DIRECTION ( 'NONE',  ( -0.000000000000000000, -1.000000000000000000, -0.000000000000000000 ) ) ;
#14343 = EDGE_CURVE ( 'NONE', #7423, #11991, #4681, .T. ) ;
#14344 = DIRECTION ( 'NONE',  ( 0.000000000000000000, 0.000000000000000000, 1.000000000000000000 ) ) ;
#14345 = CARTESIAN_POINT ( 'NONE',  ( 40.34137639590981905, 44.72187500034139163, 29.30972558990010768 ) ) ;
#14346 = CARTESIAN_POINT ( 'NONE',  ( -49.86468353124999453, 23.75937500034140015, -16.20201782572375393 ) ) ;
#14347 = FACE_OUTER_BOUND ( 'NONE', #6344, .T. ) ;
#14348 = CARTESIAN_POINT ( 'NONE',  ( 30.81806926056962936, 39.22187500034139873, -42.41743335407646498 ) ) ;
#14349 = PRODUCT_CONTEXT ( 'NONE', #2269, 'mechanical' ) ;
#14350 = CARTESIAN_POINT ( 'NONE',  ( 30.90169943749475223, 34.48125000068279888, 42.53254041760199300 ) ) ;
#14351 = CARTESIAN_POINT ( 'NONE',  ( -15.40903463028481646, 49.52187500034140299, -47.42413220539093999 ) ) ;
#14352 = DIRECTION ( 'NONE',  ( 0.000000000000000000, 0.000000000000000000, -1.000000000000000000 ) ) ;
#14353 = ORIENTED_EDGE ( 'NONE', *, *, #8383, .T. ) ;
#14354 = CARTESIAN_POINT ( 'NONE',  ( 9.631387414534489405E-15, 20.35937500034139092, 52.43083105670540789 ) ) ;
#14355 = ORIENTED_EDGE ( 'NONE', *, *, #4912, .F. ) ;
#14356 = ORIENTED_EDGE ( 'NONE', *, *, #9936, .F. ) ;
#14357 = ADVANCED_FACE ( 'NONE', ( #15702, #8225 ), #14443, .T. ) ;
#14358 = DIRECTION ( 'NONE',  ( -0.9510565162951503115, -0.3090169943749574988, 0.000000000000000000 ) ) ;
#14359 = DIRECTION ( 'NONE',  ( -0.000000000000000000, -1.000000000000000000, -0.000000000000000000 ) ) ;
#14360 = DIRECTION ( 'NONE',  ( 1.067350013832299517E-17, 0.9961946980917455452, -0.08715574274765836016 ) ) ;
#14361 = CARTESIAN_POINT ( 'NONE',  ( -3.219174618344376363E-15, 25.50000000000000355, -52.57311121191334990 ) ) ;
#14362 = CARTESIAN_POINT ( 'NONE',  ( -15.40903463028481646, 41.45937500034140299, -47.42413220539093999 ) ) ;
#14363 = CARTESIAN_POINT ( 'NONE',  ( -3.111920190527341144E-15, 25.28125000068279604, -50.00000000000000000 ) ) ;
#14364 = CARTESIAN_POINT ( 'NONE',  ( 0.5000000000000000000, 39.99285568453590400, 101.0000000000000000 ) ) ;
#14365 = PLANE ( 'NONE',  #2289 ) ;
#14366 = DIRECTION ( 'NONE',  ( 0.000000000000000000, -1.000000000000000000, 0.000000000000000000 ) ) ;
#14367 = CARTESIAN_POINT ( 'NONE',  ( 50.00000000000000711, 36.68125000068280173, 16.24598481164530739 ) ) ;
#14368 = CARTESIAN_POINT ( 'NONE',  ( -45.00000000000000000, 262.0000000000000000, -10.00000000000000178 ) ) ;
#14369 = LINE ( 'NONE', #321, #16399 ) ;
#14370 = CARTESIAN_POINT ( 'NONE',  ( 0.000000000000000000, 272.0000000000000000, 0.000000000000000000 ) ) ;
#14371 = ORIENTED_EDGE ( 'NONE', *, *, #2314, .F. ) ;
#14372 = CARTESIAN_POINT ( 'NONE',  ( 40.34137639590981195, 35.05937500034139731, -29.30972558990011834 ) ) ;
#14373 = EDGE_LOOP ( 'NONE', ( #8630, #2167, #5629, #14889 ) ) ;
#14374 = EDGE_LOOP ( 'NONE', ( #6912, #8623, #12833, #9400, #10657 ) ) ;
#14375 = DIRECTION ( 'NONE',  ( 0.000000000000000000, 0.000000000000000000, 1.000000000000000000 ) ) ;
#14376 = LINE ( 'NONE', #15881, #4438 ) ;
#14377 = CARTESIAN_POINT ( 'NONE',  ( -40.34137639590981905, 21.65937500034139518, -29.30972558990011478 ) ) ;
#14378 = VERTEX_POINT ( 'NONE', #8148 ) ;
#14379 = CARTESIAN_POINT ( 'NONE',  ( 25.00000000000000000, 307.0000000000000568, -2.499999999999997780 ) ) ;
#14380 = DIRECTION ( 'NONE',  ( 1.224646799147349509E-16, 0.000000000000000000, -1.000000000000000000 ) ) ;
#14381 = CARTESIAN_POINT ( 'NONE',  ( 50.00000000000000000, 25.00000000000000000, -6.123233995736766085E-15 ) ) ;
#14382 = CARTESIAN_POINT ( 'NONE',  ( -49.86468353124999453, 25.82187500034139305, -16.20201782572375393 ) ) ;
#14383 = CARTESIAN_POINT ( 'NONE',  ( -30.90169943749474513, 37.48125000068279888, -42.53254041760200721 ) ) ;
#14384 = CARTESIAN_POINT ( 'NONE',  ( 7.309249795462555710, 6.589106271932131165, 98.56897796993928296 ) ) ;
#14385 = CARTESIAN_POINT ( 'NONE',  ( -48.33688377893763999, 20.00000000000000355, 12.24883938693908725 ) ) ;
#14386 = CARTESIAN_POINT ( 'NONE',  ( -30.81806926056963292, 29.62187500034139376, -42.41743335407646498 ) ) ;
#14387 = CARTESIAN_POINT ( 'NONE',  ( 24.78626291527397285, 25.00000000000000355, 5.650101528493621572 ) ) ;
#14388 = CARTESIAN_POINT ( 'NONE',  ( 30.90169943749474157, 35.30000000000000426, -42.53254041760200721 ) ) ;
#14389 = CARTESIAN_POINT ( 'NONE',  ( 15.40903463028481113, 35.25937500034139305, -47.42413220539094709 ) ) ;
#14390 = CARTESIAN_POINT ( 'NONE',  ( 0.000000000000000000, 22.50000000000000000, 102.0000000000000142 ) ) ;
#14391 = VERTEX_POINT ( 'NONE', #640 ) ;
#14392 = VECTOR ( 'NONE', #5328, 1000.000000000000000 ) ;
#14393 = CARTESIAN_POINT ( 'NONE',  ( -30.81806926056963292, 29.55937500034139376, -42.41743335407646498 ) ) ;
#14394 = ORIENTED_EDGE ( 'NONE', *, *, #8730, .T. ) ;
#14395 = CARTESIAN_POINT ( 'NONE',  ( 1.112556234935474772E-14, 279.6527036446661327, -90.84711083310548929 ) ) ;
#14396 = CARTESIAN_POINT ( 'NONE',  ( -30.81806926056963292, 39.55937500034139731, -42.41743335407647209 ) ) ;
#14397 = CARTESIAN_POINT ( 'NONE',  ( 29.01527194596310721, 282.0655843567844272, 11.51527194596232206 ) ) ;
#14398 = CARTESIAN_POINT ( 'NONE',  ( -20.00000000000114042, 286.6727470533917312, 7.500000000000002665 ) ) ;
#14399 = CARTESIAN_POINT ( 'NONE',  ( -15.40903463028481646, 37.52187500034139589, -47.42413220539093999 ) ) ;
#14400 = CARTESIAN_POINT ( 'NONE',  ( 30.81806926056962936, 33.15937500034139873, -42.41743335407646498 ) ) ;
#14401 = DIRECTION ( 'NONE',  ( -3.469446951953613696E-16, 0.000000000000000000, -1.000000000000000000 ) ) ;
#14402 = CARTESIAN_POINT ( 'NONE',  ( -15.45084971874737256, 39.60000000000000142, -47.55282581475767500 ) ) ;
#14403 = CIRCLE ( 'NONE', #2998, 5.000000000000004441 ) ;
#14404 = CARTESIAN_POINT ( 'NONE',  ( -30.90169943749474868, 23.48125000068279888, -42.53254041760200721 ) ) ;
#14405 = CARTESIAN_POINT ( 'NONE',  ( -30.81806926056962226, 42.22187500034139163, 42.41743335407647919 ) ) ;
#14406 = CARTESIAN_POINT ( 'NONE',  ( 15.40903463028482356, 28.52187500034139589, 47.42413220539093999 ) ) ;
#14407 =( BOUNDED_CURVE ( )  B_SPLINE_CURVE ( 2, ( #1158, #8815, #12313, #6011, #914, #5024, #8493, #3756, #4775, #9913, #4939, #7338, #11323 ),
 .UNSPECIFIED., .F., .F. ) 
 B_SPLINE_CURVE_WITH_KNOTS ( ( 3, 2, 2, 2, 2, 2, 3 ),
 ( 0.1833333333333333481, 0.1866666666666666752, 0.1933333333333333293, 0.2000000000000000111, 0.2066666666666666652, 0.2133333333333333470, 0.2166666666666666741 ),
 .UNSPECIFIED. ) 
 CURVE ( )  GEOMETRIC_REPRESENTATION_ITEM ( )  RATIONAL_B_SPLINE_CURVE ( ( 0.9755282581475767101, 0.9755282581475768211, 1.000000000000000000, 0.9510565162951535312, 1.000000000000000000, 0.9510565162951535312, 1.000000000000000000, 0.9510565162951535312, 1.000000000000000000, 0.9510565162951535312, 1.000000000000000000, 0.9755282581475768211, 0.9755282581475768211 ) ) 
 REPRESENTATION_ITEM ( '' )  );
#14408 = CARTESIAN_POINT ( 'NONE',  ( 4.350898428888834396E-14, 37.00000000000001421, 10.00000000000000355 ) ) ;
#14409 = EDGE_LOOP ( 'NONE', ( #1272, #8697, #14758, #1896 ) ) ;
#14410 = CARTESIAN_POINT ( 'NONE',  ( -49.99999999999999289, 29.88125000068279391, 16.24598481164533226 ) ) ;
#14411 = AXIS2_PLACEMENT_3D ( 'NONE', #7002, #15716, #5437 ) ;
#14412 = ORIENTED_EDGE ( 'NONE', *, *, #10165, .F. ) ;
#14413 = CARTESIAN_POINT ( 'NONE',  ( -9.642970592016627762, 99.14870971539799882, -1.872989114519522547 ) ) ;
#14414 = DIRECTION ( 'NONE',  ( 1.000000000000000000, -1.784287003861858895E-15, 0.000000000000000000 ) ) ;
#14415 = EDGE_CURVE ( 'NONE', #13965, #1001, #5458, .T. ) ;
#14416 = CARTESIAN_POINT ( 'NONE',  ( 2.600676159226420495E-13, 31.28125000068279604, -49.99999999999999289 ) ) ;
#14417 = CARTESIAN_POINT ( 'NONE',  ( -30.81806926056962226, 44.22187500034139163, 42.41743335407647209 ) ) ;
#14418 = CARTESIAN_POINT ( 'NONE',  ( -3.210462471511496205E-15, 27.35937500034139802, -52.43083105670540789 ) ) ;
#14419 = CARTESIAN_POINT ( 'NONE',  ( -7.919222016226870942, 40.22999571913594963, 49.99999999999997158 ) ) ;
#14420 = CARTESIAN_POINT ( 'NONE',  ( 49.86468353125000164, 40.92187500034139447, -6.106662507704105588E-15 ) ) ;
#14421 = EDGE_CURVE ( 'NONE', #14922, #8698, #1119, .T. ) ;
#14423 = EDGE_CURVE ( 'NONE', #589, #13963, #15725, .T. ) ;
#14422 = VECTOR ( 'NONE', #1890, 1000.000000000000114 ) ;
#14424 = CARTESIAN_POINT ( 'NONE',  ( 49.86468353125001585, 44.82187500034138594, 16.20201782572375038 ) ) ;
#14425 = CARTESIAN_POINT ( 'NONE',  ( 7.919222016226940219, 31.44874571845315714, -49.99999999999996447 ) ) ;
#14426 = ORIENTED_EDGE ( 'NONE', *, *, #3820, .F. ) ;
#14427 = CARTESIAN_POINT ( 'NONE',  ( 49.86468353125000164, 42.92187500034140157, -6.106662507704105588E-15 ) ) ;
#14428 = VERTEX_POINT ( 'NONE', #4656 ) ;
#14429 = ORIENTED_EDGE ( 'NONE', *, *, #1841, .F. ) ;
#14430 = CARTESIAN_POINT ( 'NONE',  ( 16.79799753235259985, 27.43226914341417810, 101.0000000000000000 ) ) ;
#14431 = DIRECTION ( 'NONE',  ( 0.000000000000000000, 0.000000000000000000, 1.000000000000000000 ) ) ;
#14432 = VECTOR ( 'NONE', #7480, 1000.000000000000000 ) ;
#14433 = DIRECTION ( 'NONE',  ( 0.000000000000000000, 1.000000000000000000, 0.000000000000000000 ) ) ;
#14434 = CARTESIAN_POINT ( 'NONE',  ( -40.45084971874737789, 23.80000000000000071, -29.38926261462365730 ) ) ;
#14435 = CARTESIAN_POINT ( 'NONE',  ( -3.210462471511496205E-15, 43.35937500034138736, -52.43083105670540789 ) ) ;
#14436 = CARTESIAN_POINT ( 'NONE',  ( 0.000000000000000000, 20.00000000000000355, 0.000000000000000000 ) ) ;
#14437 = DIRECTION ( 'NONE',  ( 0.000000000000000000, 0.000000000000000000, 1.000000000000000000 ) ) ;
#14438 = CARTESIAN_POINT ( 'NONE',  ( -3.111920190527341144E-15, 43.28125000068280315, -50.00000000000000000 ) ) ;
#14439 = CARTESIAN_POINT ( 'NONE',  ( 30.90169943749475223, 48.69999999999999574, 42.53254041760199300 ) ) ;
#14440 = CARTESIAN_POINT ( 'NONE',  ( 9.657523855033129090E-15, 34.28125000068278894, 52.57311121191334990 ) ) ;
#14441 = LINE ( 'NONE', #14368, #7368 ) ;
#14442 = CARTESIAN_POINT ( 'NONE',  ( 2.600676159226420495E-13, 23.28125000068279604, -49.99999999999999289 ) ) ;
#14443 = PLANE ( 'NONE',  #2457 ) ;
#14444 = EDGE_LOOP ( 'NONE', ( #10402, #9048, #13618, #7400 ) ) ;
#14445 = AXIS2_PLACEMENT_3D ( 'NONE', #4505, #15882, #16209 ) ;
#14446 = CARTESIAN_POINT ( 'NONE',  ( 15.40903463028482356, 34.45937500034139589, 47.42413220539093999 ) ) ;
#14447 = ORIENTED_EDGE ( 'NONE', *, *, #6349, .T. ) ;
#14448 = ORIENTED_EDGE ( 'NONE', *, *, #1221, .F. ) ;
#14449 = CARTESIAN_POINT ( 'NONE',  ( 40.45084971874737079, 48.98125000068279888, -29.38926261462366440 ) ) ;
#14450 = DIRECTION ( 'NONE',  ( 0.000000000000000000, 0.000000000000000000, 1.000000000000000000 ) ) ;
#14451 = CARTESIAN_POINT ( 'NONE',  ( 40.34137639590981905, 20.65937500034139873, 29.30972558990010768 ) ) ;
#14452 = ORIENTED_EDGE ( 'NONE', *, *, #1873, .F. ) ;
#14453 = DIRECTION ( 'NONE',  ( 0.000000000000000000, 0.000000000000000000, 1.000000000000000000 ) ) ;
#14454 = CARTESIAN_POINT ( 'NONE',  ( -8.660254037844415720, 37.00000000000001421, -4.999999999999952038 ) ) ;
#14455 = CARTESIAN_POINT ( 'NONE',  ( 46.00570371104048206, 25.06239642599078365, -21.51344788172325195 ) ) ;
#14456 = VECTOR ( 'NONE', #13927, 1000.000000000000000 ) ;
#14457 = CARTESIAN_POINT ( 'NONE',  ( -3.111920190527341144E-15, 29.28125000068279604, -50.00000000000000000 ) ) ;
#14458 = CARTESIAN_POINT ( 'NONE',  ( 12.84309919097911923, 10.59908474996653460, 97.28791577635783483 ) ) ;
#14459 = CARTESIAN_POINT ( 'NONE',  ( -47.18644234407105387, 20.00000000000000355, 16.12223069495573924 ) ) ;
#14460 = CARTESIAN_POINT ( 'NONE',  ( 15.40903463028481113, 25.32187500034139660, -47.42413220539094709 ) ) ;
#14461 = CARTESIAN_POINT ( 'NONE',  ( -50.00000000000000000, 34.00000000000000000, 0.000000000000000000 ) ) ;
#14462 = CARTESIAN_POINT ( 'NONE',  ( 9.631387414534489405E-15, 24.35937500034139802, 52.43083105670540789 ) ) ;
#14463 = CARTESIAN_POINT ( 'NONE',  ( -1.240322475938754499E-13, 38.50000000000000711, 50.00000000000000000 ) ) ;
#14464 = ORIENTED_EDGE ( 'NONE', *, *, #826, .F. ) ;
#14465 = VECTOR ( 'NONE', #15675, 1000.000000000000000 ) ;
#14466 = CARTESIAN_POINT ( 'NONE',  ( -30.81806926056962226, 30.15937500034139163, 42.41743335407647209 ) ) ;
#14467 = EDGE_CURVE ( 'NONE', #4062, #9157, #11237, .T. ) ;
#14468 = VERTEX_POINT ( 'NONE', #14606 ) ;
#14469 =( GEOMETRIC_REPRESENTATION_CONTEXT ( 3 ) GLOBAL_UNCERTAINTY_ASSIGNED_CONTEXT ( ( #100 ) ) GLOBAL_UNIT_ASSIGNED_CONTEXT ( ( #13795, #7486, #6245 ) ) REPRESENTATION_CONTEXT ( 'NONE', 'WORKASPACE' ) );
#14470 = FACE_OUTER_BOUND ( 'NONE', #3548, .T. ) ;
#14471 = CARTESIAN_POINT ( 'NONE',  ( -30.81806926056962226, 40.15937500034139163, 42.41743335407647919 ) ) ;
#14472 = VECTOR ( 'NONE', #524, 1000.000000000000114 ) ;
#14473 = CARTESIAN_POINT ( 'NONE',  ( 23.39173249367787122, 283.2330659412879186, 9.195866246846582825 ) ) ;
#14474 = CARTESIAN_POINT ( 'NONE',  ( -21.01167039530930936, 284.7842439685843487, 8.005835197660418956 ) ) ;
#14475 = AXIS2_PLACEMENT_3D ( 'NONE', #9834, #3513, #2164 ) ;
#14476 = CARTESIAN_POINT ( 'NONE',  ( 40.34137639590981195, 35.12187500034139731, -29.30972558990011834 ) ) ;
#14477 = CARTESIAN_POINT ( 'NONE',  ( -49.86468353124999453, 35.75937500034139305, -16.20201782572375393 ) ) ;
#14478 = AXIS2_PLACEMENT_3D ( 'NONE', #15771, #9383, #5577 ) ;
#14479 = VECTOR ( 'NONE', #15304, 1000.000000000000000 ) ;
#14480 = CARTESIAN_POINT ( 'NONE',  ( -15.45084971874737256, 43.60000000000000142, -47.55282581475767500 ) ) ;
#14481 = CARTESIAN_POINT ( 'NONE',  ( 9.631387414534489405E-15, 32.42187500034139447, 52.43083105670540789 ) ) ;
#14482 = AXIS2_PLACEMENT_3D ( 'NONE', #10514, #1844, #10838 ) ;
#14483 = CARTESIAN_POINT ( 'NONE',  ( 40.45084971874737789, 42.80000000000000426, 29.38926261462365375 ) ) ;
#14484 = CARTESIAN_POINT ( 'NONE',  ( 15.45084971874736723, 21.18125000068279817, -47.55282581475768211 ) ) ;
#14485 = CARTESIAN_POINT ( 'NONE',  ( 30.81806926056964002, 42.62187500034139731, 42.41743335407647209 ) ) ;
#14486 = PRODUCT_DEFINITION_FORMATION_WITH_SPECIFIED_SOURCE ( 'ANY', '', #5621, .NOT_KNOWN. ) ;
#14487 = CARTESIAN_POINT ( 'NONE',  ( 30.90169943749474157, 49.29999999999999716, -42.53254041760200721 ) ) ;
#14488 = ORIENTED_EDGE ( 'NONE', *, *, #4528, .T. ) ;
#14489 = CARTESIAN_POINT ( 'NONE',  ( -30.81806926056963292, 49.55937500034139731, -42.41743335407646498 ) ) ;
#14490 = AXIS2_PLACEMENT_3D ( 'NONE', #686, #5861, #853 ) ;
#14491 = ORIENTED_EDGE ( 'NONE', *, *, #14773, .T. ) ;
#14492 = AXIS2_PLACEMENT_3D ( 'NONE', #107, #13831, #3867 ) ;
#14493 = CIRCLE ( 'NONE', #7358, 45.00000000000000000 ) ;
#14495 = CARTESIAN_POINT ( 'NONE',  ( 49.99999999999999289, 32.88125000068280457, -16.24598481164532160 ) ) ;
#14494 = AXIS2_PLACEMENT_3D ( 'NONE', #8995, #16397, #7742 ) ;
#14496 = ORIENTED_EDGE ( 'NONE', *, *, #14044, .T. ) ;
#14497 = CARTESIAN_POINT ( 'NONE',  ( 3.149380788944009968, 5.278461141749541063, 101.0000000000000000 ) ) ;
#14498 = CARTESIAN_POINT ( 'NONE',  ( 7.919222016226940219, 31.22999571913595673, -49.99999999999996447 ) ) ;
#14499 = CARTESIAN_POINT ( 'NONE',  ( 30.81806926056964002, 38.62187500034139020, 42.41743335407646498 ) ) ;
#14500 = CARTESIAN_POINT ( 'NONE',  ( -3.210462471511496205E-15, 23.35937500034139802, -52.43083105670540789 ) ) ;
#14501 = CARTESIAN_POINT ( 'NONE',  ( 14.90544456622775904, 13.31698729810792692, 101.0000000000000000 ) ) ;
#14502 = VECTOR ( 'NONE', #158, 1000.000000000000000 ) ;
#14503 = APPLICATION_PROTOCOL_DEFINITION ( 'draft international standard', 'automotive_design', 1998, #14591 ) ;
#14504 = CARTESIAN_POINT ( 'NONE',  ( 15.45084971874736723, 35.39999999999999858, -47.55282581475768211 ) ) ;
#14505 = AXIS2_PLACEMENT_3D ( 'NONE', #5061, #2447, #3713 ) ;
#14507 =( BOUNDED_CURVE ( )  B_SPLINE_CURVE ( 2, ( #1817, #6910, #11964, #10884, #8542, #16121, #4569, #9632, #10963, #7227, #12287, #11142, #3566 ),
 .UNSPECIFIED., .F., .F. ) 
 B_SPLINE_CURVE_WITH_KNOTS ( ( 3, 2, 2, 2, 2, 2, 3 ),
 ( 0.4166666666666666852, 0.4199999999999999845, 0.4266666666666666941, 0.4333333333333333481, 0.4400000000000000022, 0.4466666666666666563, 0.4500000000000000111 ),
 .UNSPECIFIED. ) 
 CURVE ( )  GEOMETRIC_REPRESENTATION_ITEM ( )  RATIONAL_B_SPLINE_CURVE ( ( 0.9755282581475768211, 0.9755282581475770431, 1.000000000000000000, 0.9510565162951535312, 1.000000000000000000, 0.9510565162951535312, 1.000000000000000000, 0.9510565162951535312, 1.000000000000000000, 0.9510565162951535312, 1.000000000000000000, 0.9755282581475765991, 0.9755282581475768211 ) ) 
 REPRESENTATION_ITEM ( '' )  );
#14506 = CONICAL_SURFACE ( 'NONE', #698, 35.00000000000000711, 0.3490658503988666728 ) ;
#14508 = CARTESIAN_POINT ( 'NONE',  ( -49.86468353124999453, 45.82187500034140015, -16.20201782572375393 ) ) ;
#14509 = PLANE ( 'NONE',  #9904 ) ;
#14510 = VERTEX_POINT ( 'NONE', #3229 ) ;
#14511 = EDGE_CURVE ( 'NONE', #7047, #14534, #9725, .T. ) ;
#14512 = CARTESIAN_POINT ( 'NONE',  ( -40.34137639590981905, 43.72187500034139873, -29.30972558990011478 ) ) ;
#14513 = ORIENTED_EDGE ( 'NONE', *, *, #2957, .F. ) ;
#14514 = ORIENTED_EDGE ( 'NONE', *, *, #5256, .F. ) ;
#14515 = EDGE_CURVE ( 'NONE', #12805, #5870, #12334, .T. ) ;
#14516 = DIRECTION ( 'NONE',  ( 0.000000000000000000, 0.000000000000000000, 1.000000000000000000 ) ) ;
#14517 = DIRECTION ( 'NONE',  ( 0.000000000000000000, 0.000000000000000000, 1.000000000000000000 ) ) ;
#14518 = CARTESIAN_POINT ( 'NONE',  ( 0.000000000000000000, 50.00000000000000000, 0.000000000000000000 ) ) ;
#14519 = LINE ( 'NONE', #13361, #14273 ) ;
#14520 = CARTESIAN_POINT ( 'NONE',  ( 49.86468353125001585, 46.75937500034140015, 16.20201782572375038 ) ) ;
#14521 = CARTESIAN_POINT ( 'NONE',  ( 15.40903463028481113, 47.25937500034140015, -47.42413220539094709 ) ) ;
#14522 = DIRECTION ( 'NONE',  ( -1.000000000000000000, 0.000000000000000000, 2.312964634635742464E-16 ) ) ;
#14523 = CARTESIAN_POINT ( 'NONE',  ( -7.919222016226934890, 34.22999571913595673, 49.99999999999996447 ) ) ;
#14524 = CONICAL_SURFACE ( 'NONE', #15596, 62.01141590572476758, 0.08726646259971666819 ) ;
#14525 = ADVANCED_FACE ( 'NONE', ( #13856 ), #13695, .F. ) ;
#14526 = DIRECTION ( 'NONE',  ( 0.000000000000000000, 0.000000000000000000, 1.000000000000000000 ) ) ;
#14527 = DIRECTION ( 'NONE',  ( 1.224646799147353207E-16, -1.000000000000000000, 0.000000000000000000 ) ) ;
#14528 = CARTESIAN_POINT ( 'NONE',  ( -2.547328955960238000E-13, 20.28125000068279959, 49.99999999999999289 ) ) ;
#14529 = LINE ( 'NONE', #5656, #6719 ) ;
#14530 = ORIENTED_EDGE ( 'NONE', *, *, #16267, .T. ) ;
#14531 = EDGE_CURVE ( 'NONE', #11153, #3858, #6982, .T. ) ;
#14532 = CARTESIAN_POINT ( 'NONE',  ( -15.40903463028481646, 31.45937500034139944, -47.42413220539093999 ) ) ;
#14533 = EDGE_LOOP ( 'NONE', ( #4333, #3733, #13220, #3034 ) ) ;
#14534 = VERTEX_POINT ( 'NONE', #6075 ) ;
#14535 = ORIENTED_EDGE ( 'NONE', *, *, #9912, .T. ) ;
#14536 = CARTESIAN_POINT ( 'NONE',  ( -40.45084971874737789, 47.58125000068280031, -29.38926261462365730 ) ) ;
#14537 = CARTESIAN_POINT ( 'NONE',  ( 9.220054415934899174E-15, 45.00000000000001421, -2.129832066681984848E-14 ) ) ;
#14538 = CARTESIAN_POINT ( 'NONE',  ( 40.34137639590981195, 25.05937500034139376, -29.30972558990011834 ) ) ;
#14539 = ORIENTED_EDGE ( 'NONE', *, *, #1354, .T. ) ;
#14540 = CARTESIAN_POINT ( 'NONE',  ( -49.99999999999999289, 48.09999999999999432, 16.24598481164533226 ) ) ;
#14541 = CARTESIAN_POINT ( 'NONE',  ( -30.00000000000000711, 282.0000000000000000, -12.49999999999999822 ) ) ;
#14542 = DIRECTION ( 'NONE',  ( 0.000000000000000000, 1.000000000000000000, 0.000000000000000000 ) ) ;
#14543 = CARTESIAN_POINT ( 'NONE',  ( -15.40903463028480580, 26.32187500034140015, 47.42413220539094709 ) ) ;
#14544 = DIRECTION ( 'NONE',  ( -0.000000000000000000, -1.000000000000000000, -0.000000000000000000 ) ) ;
#14545 = EDGE_CURVE ( 'NONE', #1879, #3153, #4913, .T. ) ;
#14546 = CARTESIAN_POINT ( 'NONE',  ( 1.157856716130699404, 5.028685516365632324, 99.10823101669018342 ) ) ;
#14547 = CARTESIAN_POINT ( 'NONE',  ( -47.74744883082067304, 20.00000000000000355, 14.37691108325808109 ) ) ;
#14548 = CARTESIAN_POINT ( 'NONE',  ( 40.34137639590981905, 22.72187500034139518, 29.30972558990010768 ) ) ;
#14549 = FACE_OUTER_BOUND ( 'NONE', #9617, .T. ) ;
#14550 = CARTESIAN_POINT ( 'NONE',  ( -49.99999999999999289, 32.10000000000000142, 16.24598481164533226 ) ) ;
#14551 = CARTESIAN_POINT ( 'NONE',  ( -49.86468353124999453, 23.95937500034138878, 16.20201782572377525 ) ) ;
#14552 = EDGE_CURVE ( 'NONE', #11668, #842, #14555, .T. ) ;
#14553 = CARTESIAN_POINT ( 'NONE',  ( -7.919222016226816763, 29.55125428154684286, -49.99999999999999289 ) ) ;
#14554 = EDGE_LOOP ( 'NONE', ( #14491, #11223, #3553, #14103 ) ) ;
#14555 =( BOUNDED_CURVE ( )  B_SPLINE_CURVE ( 2, ( #9886, #8878, #10132, #13612, #5984, #16447, #2311, #8543, #16358, #4998, #15182, #7550, #7396 ),
 .UNSPECIFIED., .F., .F. ) 
 B_SPLINE_CURVE_WITH_KNOTS ( ( 3, 2, 2, 2, 2, 2, 3 ),
 ( 0.2500000000000000000, 0.2533333333333333548, 0.2600000000000000089, 0.2666666666666666630, 0.2733333333333333171, 0.2800000000000000266, 0.2833333333333333814 ),
 .UNSPECIFIED. ) 
 CURVE ( )  GEOMETRIC_REPRESENTATION_ITEM ( )  RATIONAL_B_SPLINE_CURVE ( ( 0.9755282581475765991, 0.9755282581475765991, 1.000000000000000000, 0.9510565162951535312, 1.000000000000000000, 0.9510565162951535312, 1.000000000000000000, 0.9510565162951535312, 1.000000000000000000, 0.9510565162951535312, 1.000000000000000000, 0.9755282581475765991, 0.9755282581475768211 ) ) 
 REPRESENTATION_ITEM ( '' )  );
#14556 = UNCERTAINTY_MEASURE_WITH_UNIT (LENGTH_MEASURE( 1.000000000000000082E-05 ), #9391, 'distance_accuracy_value', 'NONE');
#14557 = CARTESIAN_POINT ( 'NONE',  ( -15.40903463028481646, 31.45937500034139944, -47.42413220539093999 ) ) ;
#14558 = ORIENTED_EDGE ( 'NONE', *, *, #10918, .F. ) ;
#14559 = FACE_OUTER_BOUND ( 'NONE', #7348, .T. ) ;
#14560 = CARTESIAN_POINT ( 'NONE',  ( 49.86468353125000164, 38.85937500034139447, -6.106662507704105588E-15 ) ) ;
#14561 = EDGE_CURVE ( 'NONE', #15028, #14214, #8027, .T. ) ;
#14562 = DIRECTION ( 'NONE',  ( 0.000000000000000000, -0.000000000000000000, 1.000000000000000000 ) ) ;
#14563 = DIRECTION ( 'NONE',  ( 0.000000000000000000, 0.000000000000000000, 1.000000000000000000 ) ) ;
#14564 = CARTESIAN_POINT ( 'NONE',  ( 30.81806926056962936, 31.22187500034139873, -42.41743335407647209 ) ) ;
#14565 = CARTESIAN_POINT ( 'NONE',  ( 49.86468353124999453, 38.95937500034139589, -16.20201782572376104 ) ) ;
#14566 = CARTESIAN_POINT ( 'NONE',  ( -40.45084971874737789, 43.80000000000000426, -29.38926261462365730 ) ) ;
#14567 = CARTESIAN_POINT ( 'NONE',  ( 49.86468353124999453, 33.02187500034139589, -16.20201782572376459 ) ) ;
#14568 = CARTESIAN_POINT ( 'NONE',  ( 50.00000000000000000, 41.00000000000000000, -6.123233995736766085E-15 ) ) ;
#14569 = CARTESIAN_POINT ( 'NONE',  ( -40.34137639590981905, 43.65937500034139163, -29.30972558990011478 ) ) ;
#14570 = CARTESIAN_POINT ( 'NONE',  ( 15.40903463028481113, 41.32187500034140015, -47.42413220539094709 ) ) ;
#14571 = CARTESIAN_POINT ( 'NONE',  ( 49.86468353124999453, 21.02187500034139589, -16.20201782572376459 ) ) ;
#14572 = ORIENTED_EDGE ( 'NONE', *, *, #2049, .T. ) ;
#14573 = CYLINDRICAL_SURFACE ( 'NONE', #3315, 50.00000000000000000 ) ;
#14574 = ORIENTED_EDGE ( 'NONE', *, *, #10387, .T. ) ;
#14575 = VERTEX_POINT ( 'NONE', #10052 ) ;
#14576 = CARTESIAN_POINT ( 'NONE',  ( 40.45084971874737789, 28.58125000068280031, 29.38926261462365375 ) ) ;
#14577 = VERTEX_POINT ( 'NONE', #14941 ) ;
#14578 = CARTESIAN_POINT ( 'NONE',  ( 7.919222016226693306, 32.33250428222964246, 50.00000000000003553 ) ) ;
#14579 = CARTESIAN_POINT ( 'NONE',  ( -40.34137639590981905, 37.72187500034139873, -29.30972558990011478 ) ) ;
#14580 = CARTESIAN_POINT ( 'NONE',  ( -30.81806926056963292, 47.62187500034139731, -42.41743335407647209 ) ) ;
#14581 = CARTESIAN_POINT ( 'NONE',  ( -5.000000000000000000, 96.75198296766782846, -7.580410092413988998 ) ) ;
#14582 = EDGE_CURVE ( 'NONE', #3234, #13411, #8621, .T. ) ;
#14583 = CONTEXT_DEPENDENT_SHAPE_REPRESENTATION ( #2168, #11564 ) ;
#14584 = CARTESIAN_POINT ( 'NONE',  ( -40.45084971874737079, 36.20000000000000284, 29.38926261462367151 ) ) ;
#14585 = CARTESIAN_POINT ( 'NONE',  ( 49.86468353125000164, 38.92187500034139447, -6.106662507704105588E-15 ) ) ;
#14586 = DIRECTION ( 'NONE',  ( 0.000000000000000000, 1.000000000000000000, 0.000000000000000000 ) ) ;
#14587 = VERTEX_POINT ( 'NONE', #12464 ) ;
#14588 = CARTESIAN_POINT ( 'NONE',  ( 49.86468353124999453, 43.02187500034138878, -16.20201782572376459 ) ) ;
#14589 = VERTEX_POINT ( 'NONE', #13936 ) ;
#14590 = ORIENTED_EDGE ( 'NONE', *, *, #4797, .T. ) ;
#14591 = APPLICATION_CONTEXT ( 'automotive_design' ) ;
#14592 = ORIENTED_EDGE ( 'NONE', *, *, #4336, .T. ) ;
#14593 = CONICAL_SURFACE ( 'NONE', #2307, 49.99999999999999289, 0.7853981633974642662 ) ;
#14594 = DIRECTION ( 'NONE',  ( -0.000000000000000000, 1.000000000000000000, -0.000000000000000000 ) ) ;
#14595 = DIRECTION ( 'NONE',  ( -0.8660254037844433705, 0.4999999999999918954, 0.000000000000000000 ) ) ;
#14596 = LINE ( 'NONE', #5645, #4255 ) ;
#14597 = MANIFOLD_SOLID_BREP ( 'Boss-Extrude1', #5227 ) ;
#14598 = DIRECTION ( 'NONE',  ( 0.1045284632676435066, 0.9945218953682744001, 0.000000000000000000 ) ) ;
#14599 = CARTESIAN_POINT ( 'NONE',  ( 30.81806926056962936, 35.15937500034139873, -42.41743335407647209 ) ) ;
#14600 = CARTESIAN_POINT ( 'NONE',  ( -30.81806926056962226, 46.15937500034139873, 42.41743335407647209 ) ) ;
#14601 = CARTESIAN_POINT ( 'NONE',  ( -3.407225380398804404, 31.38205016914259105, 101.0000000000000000 ) ) ;
#14602 = PLANE ( 'NONE',  #4702 ) ;
#14603 = DIRECTION ( 'NONE',  ( -0.000000000000000000, 1.000000000000000000, -0.000000000000000000 ) ) ;
#14604 = CARTESIAN_POINT ( 'NONE',  ( 0.5000000000000000000, 39.99999999999999289, 101.0000000000000000 ) ) ;
#14605 = CARTESIAN_POINT ( 'NONE',  ( 2.600676159226420495E-13, 33.49999999999999289, -49.99999999999999289 ) ) ;
#14606 = CARTESIAN_POINT ( 'NONE',  ( 1.293669679204937499E-13, 37.28125000068280315, -50.00000000000000000 ) ) ;
#14607 = ADVANCED_FACE ( 'NONE', ( #15107 ), #3567, .F. ) ;
#14608 = ORIENTED_EDGE ( 'NONE', *, *, #73, .F. ) ;
#14609 = CARTESIAN_POINT ( 'NONE',  ( 15.40903463028481113, 29.25937500034139660, -47.42413220539094709 ) ) ;
#14610 = VERTEX_POINT ( 'NONE', #1056 ) ;
#14611 = ORIENTED_EDGE ( 'NONE', *, *, #3039, .F. ) ;
#14612 = ORIENTED_EDGE ( 'NONE', *, *, #12442, .F. ) ;
#14613 = CARTESIAN_POINT ( 'NONE',  ( 30.90169943749474157, 45.08125000068279320, -42.53254041760200721 ) ) ;
#14614 = CARTESIAN_POINT ( 'NONE',  ( 7.919222016226827421, 47.44874571845315359, -50.00000000000000000 ) ) ;
#14615 = CARTESIAN_POINT ( 'NONE',  ( 17.50000000000000000, 22.50000000000000355, 102.0000000000000142 ) ) ;
#14616 = EDGE_LOOP ( 'NONE', ( #3618, #7421, #10635, #15502 ) ) ;
#14617 = CARTESIAN_POINT ( 'NONE',  ( -30.90169943749474513, 27.48125000068279888, -42.53254041760200721 ) ) ;
#14618 = CYLINDRICAL_SURFACE ( 'NONE', #942, 50.00000000000000000 ) ;
#14619 = CARTESIAN_POINT ( 'NONE',  ( 24.78626291527397285, 40.00000000000000711, 5.650101528493618908 ) ) ;
#14620 = DIRECTION ( 'NONE',  ( -0.000000000000000000, -1.000000000000000000, -0.000000000000000000 ) ) ;
#14621 = CARTESIAN_POINT ( 'NONE',  ( 9.220054415934899174E-15, 45.00000000000001421, -2.129832066681984848E-14 ) ) ;
#14622 = EDGE_CURVE ( 'NONE', #860, #10405, #8792, .T. ) ;
#14623 = CARTESIAN_POINT ( 'NONE',  ( -15.45084971874737256, 47.60000000000000142, -47.55282581475767500 ) ) ;
#14624 = CARTESIAN_POINT ( 'NONE',  ( 6.123233995736766085E-15, 20.00000000000000355, -50.00000000000000000 ) ) ;
#14625 = DIRECTION ( 'NONE',  ( 0.000000000000000000, 1.000000000000000000, 0.000000000000000000 ) ) ;
#14626 = CARTESIAN_POINT ( 'NONE',  ( 15.40903463028482356, 20.52187500034139589, 47.42413220539093999 ) ) ;
#14627 = DIRECTION ( 'NONE',  ( 0.2079116908177531253, 0.9781476007338069101, 0.000000000000000000 ) ) ;
#14628 = EDGE_CURVE ( 'NONE', #306, #15764, #14024, .T. ) ;
#14629 = CARTESIAN_POINT ( 'NONE',  ( -15.45084971874736368, 36.39999999999999858, 47.55282581475768211 ) ) ;
#14630 = CARTESIAN_POINT ( 'NONE',  ( 49.86468353125000164, 28.85937500034139802, -6.106662507704105588E-15 ) ) ;
#14631 = EDGE_CURVE ( 'NONE', #5127, #1863, #10646, .T. ) ;
#14632 = CARTESIAN_POINT ( 'NONE',  ( -30.81806926056962226, 48.15937500034139873, 42.41743335407647919 ) ) ;
#14633 = VERTEX_POINT ( 'NONE', #9047 ) ;
#14634 = EDGE_CURVE ( 'NONE', #14047, #16188, #16263, .T. ) ;
#14635 = DIRECTION ( 'NONE',  ( 0.000000000000000000, 0.000000000000000000, 1.000000000000000000 ) ) ;
#14636 = ORIENTED_EDGE ( 'NONE', *, *, #14561, .F. ) ;
#14637 = CYLINDRICAL_SURFACE ( 'NONE', #8141, 50.00000000000000000 ) ;
#14638 = CARTESIAN_POINT ( 'NONE',  ( -40.34137639590981905, 39.65937500034139873, -29.30972558990011478 ) ) ;
#14639 = DIRECTION ( 'NONE',  ( 0.3535533905932773391, -0.7071067811865463515, 0.6123724356957938042 ) ) ;
#14640 = DIRECTION ( 'NONE',  ( 1.000000000000000000, -0.000000000000000000, 0.000000000000000000 ) ) ;
#14641 = CARTESIAN_POINT ( 'NONE',  ( 49.86468353125001585, 30.82187500034139660, 16.20201782572375038 ) ) ;
#14642 = CARTESIAN_POINT ( 'NONE',  ( 49.86468353125000164, 28.85937500034139802, -6.106662507704105588E-15 ) ) ;
#14643 = CARTESIAN_POINT ( 'NONE',  ( 30.90169943749473802, 27.08125000068280031, -42.53254041760200721 ) ) ;
#14644 = CARTESIAN_POINT ( 'NONE',  ( -15.40903463028481646, 31.52187500034139944, -47.42413220539093999 ) ) ;
#14645 = CARTESIAN_POINT ( 'NONE',  ( -2.499999999999999556, 242.0000000000000853, -49.17157287525380127 ) ) ;
#14646 = CARTESIAN_POINT ( 'NONE',  ( -40.34137639590981195, 42.05937500034139731, 29.30972558990012189 ) ) ;
#14647 = CARTESIAN_POINT ( 'NONE',  ( 30.81806926056962936, 39.22187500034139873, -42.41743335407647209 ) ) ;
#14648 = CARTESIAN_POINT ( 'NONE',  ( 40.34137639590981905, 20.72187500034139873, 29.30972558990010768 ) ) ;
#14649 = EDGE_CURVE ( 'NONE', #1407, #15190, #6192, .T. ) ;
#14650 = EDGE_LOOP ( 'NONE', ( #5051, #4295, #2248, #15859 ) ) ;
#14651 = CARTESIAN_POINT ( 'NONE',  ( -49.86468353124999453, 47.95937500034138878, 16.20201782572377169 ) ) ;
#14652 = ORIENTED_EDGE ( 'NONE', *, *, #14933, .T. ) ;
#14653 = EDGE_CURVE ( 'NONE', #11207, #8062, #2639, .T. ) ;
#14654 = CARTESIAN_POINT ( 'NONE',  ( -49.99999999999999289, 31.88125000068280102, 16.24598481164533226 ) ) ;
#14655 = ORIENTED_EDGE ( 'NONE', *, *, #6067, .F. ) ;
#14656 =( GEOMETRIC_REPRESENTATION_CONTEXT ( 3 ) GLOBAL_UNCERTAINTY_ASSIGNED_CONTEXT ( ( #7100 ) ) GLOBAL_UNIT_ASSIGNED_CONTEXT ( ( #976, #1133, #4752 ) ) REPRESENTATION_CONTEXT ( 'NONE', 'WORKASPACE' ) );
#14657 = CARTESIAN_POINT ( 'NONE',  ( -30.90169943749474513, 33.48125000068279888, -42.53254041760200721 ) ) ;
#14658 = CARTESIAN_POINT ( 'NONE',  ( -3.210462471511496205E-15, 39.42187500034139447, -52.43083105670540789 ) ) ;
#14659 = CARTESIAN_POINT ( 'NONE',  ( -15.40903463028481646, 47.52187500034139589, -47.42413220539093999 ) ) ;
#14660 = CARTESIAN_POINT ( 'NONE',  ( 9.253960653386475815E-15, 98.25246584726779986, -9.080892972013931086 ) ) ;
#14661 = CARTESIAN_POINT ( 'NONE',  ( -3.210462471511496205E-15, 25.42187500034139092, -52.43083105670540789 ) ) ;
#14662 = CARTESIAN_POINT ( 'NONE',  ( -40.45084971874737079, 38.20000000000000284, 29.38926261462367151 ) ) ;
#14663 = CARTESIAN_POINT ( 'NONE',  ( 30.81806926056962936, 41.22187500034139873, -42.41743335407647209 ) ) ;
#14664 = CARTESIAN_POINT ( 'NONE',  ( -45.00000000000000000, 262.0000000000000000, 0.000000000000000000 ) ) ;
#14665 = VERTEX_POINT ( 'NONE', #1385 ) ;
#14666 = VECTOR ( 'NONE', #14304, 1000.000000000000227 ) ;
#14667 = CARTESIAN_POINT ( 'NONE',  ( -15.40903463028480580, 44.32187500034140015, 47.42413220539094709 ) ) ;
#14668 = VERTEX_POINT ( 'NONE', #1635 ) ;
#14669 = VERTEX_POINT ( 'NONE', #1471 ) ;
#14670 = EDGE_CURVE ( 'NONE', #5931, #15550, #7247, .T. ) ;
#14671 = VERTEX_POINT ( 'NONE', #12704 ) ;
#14672 = EDGE_CURVE ( 'NONE', #7881, #11148, #2181, .T. ) ;
#14673 = CARTESIAN_POINT ( 'NONE',  ( -50.00000000000000000, 39.78125000068279604, 0.000000000000000000 ) ) ;
#14674 = B_SPLINE_CURVE_WITH_KNOTS ( 'NONE', 3,
 ( #7732, #12799, #15124, #6493 ),
 .UNSPECIFIED., .F., .F.,
 ( 4, 4 ),
 ( 2.829004760683498992E-07, 0.001414802801989366787 ),
 .UNSPECIFIED. ) ;
#14675 = DIRECTION ( 'NONE',  ( -0.000000000000000000, -1.000000000000000000, -0.000000000000000000 ) ) ;
#14676 = CARTESIAN_POINT ( 'NONE',  ( -7.919222016226818539, 49.55125428154685352, -49.99999999999999289 ) ) ;
#14677 = CARTESIAN_POINT ( 'NONE',  ( 2.500000000000000000, 247.0000000000000284, -47.99999999999999289 ) ) ;
#14678 = CARTESIAN_POINT ( 'NONE',  ( -3.210462471511496205E-15, 35.35937500034140157, -52.43083105670540789 ) ) ;
#14679 = CARTESIAN_POINT ( 'NONE',  ( 9.631387414534489405E-15, 48.35937500034139447, 52.43083105670540789 ) ) ;
#14680 = CARTESIAN_POINT ( 'NONE',  ( -2.499999999999999556, 247.0000000000000568, 49.17157287525380127 ) ) ;
#14681 = VECTOR ( 'NONE', #12479, 1000.000000000000114 ) ;
#14682 = DIRECTION ( 'NONE',  ( 0.000000000000000000, -1.000000000000000000, 0.000000000000000000 ) ) ;
#14683 = CYLINDRICAL_SURFACE ( 'NONE', #1690, 9.080892972013911546 ) ;
#14684 = CARTESIAN_POINT ( 'NONE',  ( 6.123233995736766085E-15, 20.00000000000000355, -50.00000000000000000 ) ) ;
#14685 = CARTESIAN_POINT ( 'NONE',  ( 15.45084971874737789, 40.60000000000000142, 47.55282581475767500 ) ) ;
#14686 = CARTESIAN_POINT ( 'NONE',  ( -1.240322475938754499E-13, 36.50000000000000711, 50.00000000000000000 ) ) ;
#14687 = APPLICATION_CONTEXT ( 'automotive_design' ) ;
#14688 = EDGE_LOOP ( 'NONE', ( #2188, #8517, #16448, #9013 ) ) ;
#14689 = CARTESIAN_POINT ( 'NONE',  ( -15.40903463028480580, 32.25937500034140015, 47.42413220539094709 ) ) ;
#14690 = VERTEX_POINT ( 'NONE', #2801 ) ;
#14691 = VERTEX_POINT ( 'NONE', #15435 ) ;
#14692 = ORIENTED_EDGE ( 'NONE', *, *, #9148, .F. ) ;
#14693 = VECTOR ( 'NONE', #9334, 1000.000000000000000 ) ;
#14694 = VECTOR ( 'NONE', #13796, 1000.000000000000000 ) ;
#14695 = CARTESIAN_POINT ( 'NONE',  ( 49.99999999999999289, 44.88125000068279036, -16.24598481164532160 ) ) ;
#14696 = CARTESIAN_POINT ( 'NONE',  ( 30.90169943749473802, 47.29999999999999716, -42.53254041760200721 ) ) ;
#14697 = ORIENTED_EDGE ( 'NONE', *, *, #7178, .T. ) ;
#14698 = FACE_OUTER_BOUND ( 'NONE', #5487, .T. ) ;
#14699 = CARTESIAN_POINT ( 'NONE',  ( -7.500000000000000000, 40.00000000000000711, -39.29058411375427795 ) ) ;
#14700 = DIRECTION ( 'NONE',  ( 1.000000000000000000, 0.000000000000000000, -0.000000000000000000 ) ) ;
#14701 = LINE ( 'NONE', #6999, #6761 ) ;
#14702 = DIRECTION ( 'NONE',  ( 0.000000000000000000, 0.000000000000000000, 1.000000000000000000 ) ) ;
#14703 = CARTESIAN_POINT ( 'NONE',  ( -1.240322475938754499E-13, 38.50000000000000711, 50.00000000000000000 ) ) ;
#14704 = CARTESIAN_POINT ( 'NONE',  ( -45.87472660798568569, 20.00000000000000355, 19.54543171153602188 ) ) ;
#14705 = PLANE ( 'NONE',  #7874 ) ;
#14706 = CARTESIAN_POINT ( 'NONE',  ( -25.00000000000000355, 307.0000000000000568, -2.499999999999998668 ) ) ;
#14707 = CARTESIAN_POINT ( 'NONE',  ( -30.90169943749474868, 25.69999999999999929, -42.53254041760200721 ) ) ;
#14708 = CARTESIAN_POINT ( 'NONE',  ( 15.40903463028481113, 25.25937500034139660, -47.42413220539094709 ) ) ;
#14709 = CARTESIAN_POINT ( 'NONE',  ( -3.210462471511496205E-15, 49.35937500034138736, -52.43083105670540789 ) ) ;
#14710 = ORIENTED_EDGE ( 'NONE', *, *, #3090, .T. ) ;
#14711 = EDGE_CURVE ( 'NONE', #7047, #11303, #6730, .T. ) ;
#14712 = PRODUCT_DEFINITION_CONTEXT ( 'detailed design', #3244, 'design' ) ;
#14713 = CARTESIAN_POINT ( 'NONE',  ( -3.111920190527341144E-15, 45.50000000000000000, -50.00000000000000000 ) ) ;
#14714 = ORIENTED_EDGE ( 'NONE', *, *, #11120, .T. ) ;
#14715 = CARTESIAN_POINT ( 'NONE',  ( 0.000000000000000000, 262.0000000000000000, 0.000000000000000000 ) ) ;
#14716 = CARTESIAN_POINT ( 'NONE',  ( 49.86468353124999453, 34.95937500034138878, -16.20201782572376459 ) ) ;
#14717 = CIRCLE ( 'NONE', #8898, 42.00000000000000711 ) ;
#14718 = CARTESIAN_POINT ( 'NONE',  ( 10.69075041230586365, 8.636095224584757091, 101.0000000000000000 ) ) ;
#14719 = CARTESIAN_POINT ( 'NONE',  ( 8.446640517145639571E-15, 28.28125000068279959, 50.00000000000000000 ) ) ;
#14720 = ADVANCED_FACE ( 'NONE', ( #1558 ), #6652, .F. ) ;
#14721 = CYLINDRICAL_SURFACE ( 'NONE', #5497, 50.00000000000000000 ) ;
#14722 = CARTESIAN_POINT ( 'NONE',  ( 40.34137639590981195, 31.12187500034139731, -29.30972558990011834 ) ) ;
#14723 = CARTESIAN_POINT ( 'NONE',  ( 30.81806926056964002, 26.55937500034139376, 42.41743335407646498 ) ) ;
#14724 = CARTESIAN_POINT ( 'NONE',  ( 9.642970592016636644, 99.14870971539799882, 1.872989114519530984 ) ) ;
#14725 = CARTESIAN_POINT ( 'NONE',  ( -49.86468353125000164, 27.92187500034139447, 0.000000000000000000 ) ) ;
#14726 = CARTESIAN_POINT ( 'NONE',  ( 15.39925740754319605, 14.18658485962441240, 101.0000000000000000 ) ) ;
#14727 = EDGE_CURVE ( 'NONE', #8593, #12133, #10458, .T. ) ;
#14728 = CARTESIAN_POINT ( 'NONE',  ( -40.34137639590981195, 44.05937500034139731, 29.30972558990012189 ) ) ;
#14729 = CARTESIAN_POINT ( 'NONE',  ( -40.34137639590981905, 35.72187500034139163, -29.30972558990011478 ) ) ;
#14730 = AXIS2_PLACEMENT_3D ( 'NONE', #4484, #14847, #14595 ) ;
#14731 = CARTESIAN_POINT ( 'NONE',  ( -49.99999999999999289, 49.89999999999999147, -16.24598481164531449 ) ) ;
#14732 = ORIENTED_EDGE ( 'NONE', *, *, #1637, .T. ) ;
#14733 = EDGE_CURVE ( 'NONE', #15028, #14319, #15514, .T. ) ;
#14734 = CARTESIAN_POINT ( 'NONE',  ( -40.34137639590981905, 39.65937500034139873, -29.30972558990011478 ) ) ;
#14735 = VERTEX_POINT ( 'NONE', #7639 ) ;
#14736 = CARTESIAN_POINT ( 'NONE',  ( -15.45084971874737256, 25.38125000068279746, -47.55282581475767500 ) ) ;
#14737 = ORIENTED_EDGE ( 'NONE', *, *, #14649, .F. ) ;
#14738 = VECTOR ( 'NONE', #11524, 1000.000000000000114 ) ;
#14739 = CIRCLE ( 'NONE', #9444, 7.732050807568878525 ) ;
#14740 = CARTESIAN_POINT ( 'NONE',  ( -2.547328955960238000E-13, 34.50000000000000000, 49.99999999999999289 ) ) ;
#14741 = CARTESIAN_POINT ( 'NONE',  ( -30.81806926056963292, 43.62187500034139020, -42.41743335407646498 ) ) ;
#14742 = CARTESIAN_POINT ( 'NONE',  ( 40.34137639590981195, 21.05937500034139376, -29.30972558990011834 ) ) ;
#14743 = AXIS2_PLACEMENT_3D ( 'NONE', #16273, #7792, #298 ) ;
#14744 = CARTESIAN_POINT ( 'NONE',  ( 7.500000000000000000, 25.00000000000000355, -39.29058411375427795 ) ) ;
#14745 =( BOUNDED_CURVE ( )  B_SPLINE_CURVE ( 2, ( #14713, #9837, #2003, #13560, #16150, #13640, #9757, #6102, #8496, #841, #9917, #3516, #12491 ),
 .UNSPECIFIED., .F., .F. ) 
 B_SPLINE_CURVE_WITH_KNOTS ( ( 3, 2, 2, 2, 2, 2, 3 ),
 ( 0.1499999999999999944, 0.1533333333333333215, 0.1600000000000000033, 0.1666666666666666574, 0.1733333333333333393, 0.1799999999999999933, 0.1833333333333333481 ),
 .UNSPECIFIED. ) 
 CURVE ( )  GEOMETRIC_REPRESENTATION_ITEM ( )  RATIONAL_B_SPLINE_CURVE ( ( 0.9755282581475768211, 0.9755282581475768211, 1.000000000000000000, 0.9510565162951535312, 1.000000000000000000, 0.9510565162951535312, 1.000000000000000000, 0.9510565162951535312, 1.000000000000000000, 0.9510565162951535312, 1.000000000000000000, 0.9755282581475765991, 0.9755282581475767101 ) ) 
 REPRESENTATION_ITEM ( '' )  );
#14746 = CARTESIAN_POINT ( 'NONE',  ( -15.40903463028481646, 21.52187500034139589, -47.42413220539093999 ) ) ;
#14747 = CARTESIAN_POINT ( 'NONE',  ( 40.45084971874737079, 34.98125000068279888, -29.38926261462366440 ) ) ;
#14748 = CARTESIAN_POINT ( 'NONE',  ( -49.99999999999999289, 38.10000000000000142, 16.24598481164533226 ) ) ;
#14749 = CARTESIAN_POINT ( 'NONE',  ( -49.86468353124999453, 37.82187500034139305, -16.20201782572375393 ) ) ;
#14750 = AXIS2_PLACEMENT_3D ( 'NONE', #13655, #4793, #6114 ) ;
#14751 = CARTESIAN_POINT ( 'NONE',  ( -27.40717431545314042, 282.1599167565163384, -11.20358715772689351 ) ) ;
#14752 = AXIS2_PLACEMENT_3D ( 'NONE', #16065, #5940, #4697 ) ;
#14753 = AXIS2_PLACEMENT_3D ( 'NONE', #3927, #11731, #1256 ) ;
#14754 = EDGE_LOOP ( 'NONE', ( #8194, #2376, #5742 ) ) ;
#14756 = ADVANCED_FACE ( 'NONE', ( #378 ), #5480, .T. ) ;
#14755 = AXIS2_PLACEMENT_3D ( 'NONE', #6177, #4944, #14972 ) ;
#14757 = CARTESIAN_POINT ( 'NONE',  ( 40.34137639590981195, 43.12187500034139731, -29.30972558990011834 ) ) ;
#14758 = ORIENTED_EDGE ( 'NONE', *, *, #5123, .F. ) ;
#14759 = ORIENTED_EDGE ( 'NONE', *, *, #4797, .F. ) ;
#14760 = ORIENTED_EDGE ( 'NONE', *, *, #16030, .T. ) ;
#14761 = DIRECTION ( 'NONE',  ( 0.000000000000000000, 0.000000000000000000, 1.000000000000000000 ) ) ;
#14762 = CARTESIAN_POINT ( 'NONE',  ( 0.000000000000000000, 22.50000000000000000, 100.0000000000000000 ) ) ;
#14763 = CARTESIAN_POINT ( 'NONE',  ( -7.919222016226688865, 21.33250428222963890, -50.00000000000003553 ) ) ;
#14764 = FACE_OUTER_BOUND ( 'NONE', #8989, .T. ) ;
#14765 = VECTOR ( 'NONE', #16318, 1000.000000000000114 ) ;
#14766 = CARTESIAN_POINT ( 'NONE',  ( -30.81806926056963292, 35.55937500034139020, -42.41743335407647209 ) ) ;
#14767 = CARTESIAN_POINT ( 'NONE',  ( 1.084250397222511456E-14, 50.00000000000000000, 85.01963570546854498 ) ) ;
#14768 = LINE ( 'NONE', #11044, #9815 ) ;
#14769 = AXIS2_PLACEMENT_3D ( 'NONE', #7180, #5935, #10999 ) ;
#14770 = DIRECTION ( 'NONE',  ( 0.000000000000000000, 0.000000000000000000, 1.000000000000000000 ) ) ;
#14771 = CARTESIAN_POINT ( 'NONE',  ( 9.297345850538470396E-15, 92.00000000000001421, -14.08089297201393109 ) ) ;
#14772 = CARTESIAN_POINT ( 'NONE',  ( 12.66515988160610107, 34.57657754388035443, 101.0000000000000000 ) ) ;
#14773 = EDGE_CURVE ( 'NONE', #10689, #10428, #2559, .T. ) ;
#14774 = DIRECTION ( 'NONE',  ( 2.312964634635742464E-16, 0.000000000000000000, -1.000000000000000000 ) ) ;
#14775 = ORIENTED_EDGE ( 'NONE', *, *, #5200, .F. ) ;
#14776 = CARTESIAN_POINT ( 'NONE',  ( 49.86468353125001585, 30.75937500034139305, 16.20201782572375038 ) ) ;
#14777 = ORIENTED_EDGE ( 'NONE', *, *, #3607, .F. ) ;
#14778 = VERTEX_POINT ( 'NONE', #3294 ) ;
#14779 = ORIENTED_EDGE ( 'NONE', *, *, #11697, .F. ) ;
#14780 = AXIS2_PLACEMENT_3D ( 'NONE', #5257, #16371, #16455 ) ;
#14781 = CARTESIAN_POINT ( 'NONE',  ( 9.657523855033129090E-15, 44.28125000068280315, 52.57311121191334990 ) ) ;
#14782 = CARTESIAN_POINT ( 'NONE',  ( 40.45084971874737079, 47.20000000000000284, -29.38926261462366440 ) ) ;
#14783 = DIRECTION ( 'NONE',  ( -0.000000000000000000, -0.000000000000000000, -1.000000000000000000 ) ) ;
#14784 = ORIENTED_EDGE ( 'NONE', *, *, #14531, .T. ) ;
#14785 = DIRECTION ( 'NONE',  ( 0.3420201433256697676, -0.6644630243886755494, -0.6644630243886733290 ) ) ;
#14786 = FACE_OUTER_BOUND ( 'NONE', #1721, .T. ) ;
#14787 = AXIS2_PLACEMENT_3D ( 'NONE', #769, #5859, #13491 ) ;
#14788 = DIRECTION ( 'NONE',  ( -0.000000000000000000, 1.000000000000000000, -0.000000000000000000 ) ) ;
#14789 = DIRECTION ( 'NONE',  ( 0.000000000000000000, 0.000000000000000000, 1.000000000000000000 ) ) ;
#14790 = PLANE ( 'NONE',  #14951 ) ;
#14791 = FACE_BOUND ( 'NONE', #6989, .T. ) ;
#14792 = CARTESIAN_POINT ( 'NONE',  ( 30.90169943749473802, 39.30000000000000426, -42.53254041760200721 ) ) ;
#14793 = CARTESIAN_POINT ( 'NONE',  ( -7.919222016226752814, 41.55125428154683931, -50.00000000000000711 ) ) ;
#14794 = CARTESIAN_POINT ( 'NONE',  ( 15.40903463028482356, 22.52187500034139589, 47.42413220539093999 ) ) ;
#14795 = LINE ( 'NONE', #5761, #3120 ) ;
#14796 = CARTESIAN_POINT ( 'NONE',  ( -40.45084971874737789, 29.80000000000000071, -29.38926261462365730 ) ) ;
#14797 = CARTESIAN_POINT ( 'NONE',  ( -30.81806926056962226, 26.15937500034139163, 42.41743335407647919 ) ) ;
#14798 = DIRECTION ( 'NONE',  ( -0.000000000000000000, 1.000000000000000000, -0.000000000000000000 ) ) ;
#14799 = CARTESIAN_POINT ( 'NONE',  ( -7.919222016226934890, 30.44874571845316069, 49.99999999999996447 ) ) ;
#14800 = ORIENTED_EDGE ( 'NONE', *, *, #15871, .T. ) ;
#14801 = CARTESIAN_POINT ( 'NONE',  ( -20.00000000000000355, 307.0000000000000568, 7.500000000000001776 ) ) ;
#14802 = CIRCLE ( 'NONE', #11116, 5.000000000000000000 ) ;
#14803 = EDGE_LOOP ( 'NONE', ( #14031, #7945, #11015, #98 ) ) ;
#14804 = CARTESIAN_POINT ( 'NONE',  ( 9.500222237632415911, 22.00424054664152607, 102.0000000000000142 ) ) ;
#14805 = CARTESIAN_POINT ( 'NONE',  ( 49.86468353125001585, 34.75937500034139305, 16.20201782572375038 ) ) ;
#14806 = EDGE_CURVE ( 'NONE', #15793, #15674, #3840, .T. ) ;
#14807 = EDGE_CURVE ( 'NONE', #8209, #4375, #12812, .T. ) ;
#14808 = DIRECTION ( 'NONE',  ( 0.000000000000000000, 0.000000000000000000, -1.000000000000000000 ) ) ;
#14809 = DIRECTION ( 'NONE',  ( -0.3090169943749448977, -0.9510565162951543083, 0.000000000000000000 ) ) ;
#14810 = DIRECTION ( 'NONE',  ( 0.000000000000000000, 0.9961946980917455452, 0.08715574274765836016 ) ) ;
#14811 = DIRECTION ( 'NONE',  ( 0.000000000000000000, -1.000000000000000000, 0.000000000000000000 ) ) ;
#14812 = CARTESIAN_POINT ( 'NONE',  ( -49.86468353124999453, 32.02187500034139589, 16.20201782572377525 ) ) ;
#14813 = CARTESIAN_POINT ( 'NONE',  ( 15.40903463028481113, 31.25937500034140015, -47.42413220539094709 ) ) ;
#14814 = CARTESIAN_POINT ( 'NONE',  ( -30.90169943749473447, 36.29999999999999716, 42.53254041760200721 ) ) ;
#14815 = CARTESIAN_POINT ( 'NONE',  ( -49.86468353124999453, 31.82187500034139305, -16.20201782572375393 ) ) ;
#14816 = CARTESIAN_POINT ( 'NONE',  ( 7.919222016226940219, 33.44874571845316069, -49.99999999999996447 ) ) ;
#14817 = CARTESIAN_POINT ( 'NONE',  ( -49.86468353124999453, 45.95937500034138878, 16.20201782572377525 ) ) ;
#14818 = CARTESIAN_POINT ( 'NONE',  ( 49.86468353125001585, 36.82187500034140015, 16.20201782572375038 ) ) ;
#14819 = CARTESIAN_POINT ( 'NONE',  ( -49.86468353125000164, 19.92187500034139447, 0.000000000000000000 ) ) ;
#14820 = ADVANCED_FACE ( 'NONE', ( #8206 ), #14509, .F. ) ;
#14821 = PRODUCT_DEFINITION ( 'UNKNOWN', '', #11054, #14236 ) ;
#14822 = ORIENTED_EDGE ( 'NONE', *, *, #5901, .T. ) ;
#14823 = CARTESIAN_POINT ( 'NONE',  ( -30.81806926056962226, 42.15937500034139163, 42.41743335407647209 ) ) ;
#14824 = VERTEX_POINT ( 'NONE', #13274 ) ;
#14825 = CARTESIAN_POINT ( 'NONE',  ( -30.90169943749473802, 26.08125000068279320, 42.53254041760200721 ) ) ;
#14826 = CONICAL_SURFACE ( 'NONE', #7677, 16.50000000000000711, 0.7853981633974447263 ) ;
#14827 = ORIENTED_EDGE ( 'NONE', *, *, #3093, .F. ) ;
#14828 = DIRECTION ( 'NONE',  ( 0.000000000000000000, 0.000000000000000000, 1.000000000000000000 ) ) ;
#14829 = CARTESIAN_POINT ( 'NONE',  ( -49.86468353124999453, 41.82187500034140015, -16.20201782572375393 ) ) ;
#14830 = CARTESIAN_POINT ( 'NONE',  ( 9.631387414534489405E-15, 48.42187500034140157, 52.43083105670540789 ) ) ;
#14831 = CARTESIAN_POINT ( 'NONE',  ( 50.00000000000000711, 40.89999999999999858, 16.24598481164530739 ) ) ;
#14832 = ADVANCED_FACE ( 'NONE', ( #9541 ), #4599, .T. ) ;
#14833 = CARTESIAN_POINT ( 'NONE',  ( 40.34137639590981905, 26.72187500034139518, 29.30972558990010768 ) ) ;
#14834 = CARTESIAN_POINT ( 'NONE',  ( -49.99999999999999289, 31.68125000068279462, -16.24598481164531449 ) ) ;
#14835 = CIRCLE ( 'NONE', #16182, 9.080892972013911546 ) ;
#14836 = CARTESIAN_POINT ( 'NONE',  ( -3.210462471511496205E-15, 43.42187500034140157, -52.43083105670540789 ) ) ;
#14837 = CARTESIAN_POINT ( 'NONE',  ( 0.000000000000000000, 52.00000000000000711, -42.00000000000000711 ) ) ;
#14838 = ORIENTED_EDGE ( 'NONE', *, *, #15040, .T. ) ;
#14839 = CARTESIAN_POINT ( 'NONE',  ( -30.81806926056963292, 35.62187500034140442, -42.41743335407647209 ) ) ;
#14840 = EDGE_CURVE ( 'NONE', #2743, #860, #11758, .T. ) ;
#14841 = CARTESIAN_POINT ( 'NONE',  ( -49.99999999999999289, 43.88125000068279746, 16.24598481164533226 ) ) ;
#14842 = ORIENTED_EDGE ( 'NONE', *, *, #15660, .T. ) ;
#14843 = ORIENTED_EDGE ( 'NONE', *, *, #512, .F. ) ;
#14844 = EDGE_CURVE ( 'NONE', #14665, #75, #8312, .T. ) ;
#14845 = ORIENTED_EDGE ( 'NONE', *, *, #1295, .F. ) ;
#14846 = CARTESIAN_POINT ( 'NONE',  ( -15.45084971874736368, 40.18125000068280173, 47.55282581475768211 ) ) ;
#14847 = DIRECTION ( 'NONE',  ( 0.4999999999999918954, 0.8660254037844433705, 0.000000000000000000 ) ) ;
#14848 =( BOUNDED_SURFACE ( )  B_SPLINE_SURFACE ( 3, 2, ( 
 ( #9018, #3863, #11671 ),
 ( #13002, #12680, #2860 ),
 ( #5208, #12758, #11506 ),
 ( #14154, #103, #5131 ),
 ( #15484, #5375, #5297 ),
 ( #7929, #9179, #10266 ),
 ( #190, #2770, #10429 ),
 ( #15326, #2612, #270 ),
 ( #1355, #3945, #7688 ),
 ( #14239, #10345, #14074 ),
 ( #11591, #4108, #1528 ),
 ( #1606, #16419, #2689 ),
 ( #25, #11433, #1277 ),
 ( #15409, #4026, #6528 ),
 ( #7764, #12835, #7845 ),
 ( #3783, #11354, #6367 ),
 ( #5054, #8933, #9096 ),
 ( #10105, #6447, #10184 ) ),
 .UNSPECIFIED., .F., .F., .F. ) 
 B_SPLINE_SURFACE_WITH_KNOTS ( ( 4, 2, 2, 2, 2, 2, 2, 2, 4 ),
 ( 3, 3 ),
 ( 4.712388980384689674, 4.908738521234051966, 5.105088062083414258, 5.301437602932775661, 5.497787143782137953, 5.694136684631500245, 5.890486225480861648, 6.086835766330223940, 6.283185307179586232 ),
 ( 0.000000000000000000, 1.000000000000000000 ),
 .UNSPECIFIED. ) 
 GEOMETRIC_REPRESENTATION_ITEM ( )  RATIONAL_B_SPLINE_SURFACE ( (
 ( 1.000000000000000000, 1.000000000000000000, 1.000000000000000000),
 ( 1.000000000000000000, 1.000000000000000000, 1.000000000000000000),
 ( 1.000000000000000000, 0.9967613244521382754, 1.000000000000000000),
 ( 1.000000000000000000, 0.9841171504956023330, 1.000000000000000000),
 ( 1.000000000000000000, 0.9747108043452729076, 1.000000000000000000),
 ( 1.000000000000000000, 0.9506740354170398755, 1.000000000000000000),
 ( 1.000000000000000000, 0.9360421842396995373, 1.000000000000000000),
 ( 1.000000000000000000, 0.9031650994466967619, 1.000000000000000000),
 ( 1.000000000000000000, 0.8849191470849313568, 1.000000000000000000),
 ( 1.000000000000000000, 0.8471316604839480569, 1.000000000000000000),
 ( 1.000000000000000000, 0.8275942695270729343, 1.000000000000000000),
 ( 1.000000000000000000, 0.7902180087162717914, 1.000000000000000000),
 ( 1.000000000000000000, 0.7723968217384142854, 1.000000000000000000),
 ( 1.000000000000000000, 0.7418334179587914301, 1.000000000000000000),
 ( 1.000000000000000000, 0.7291288939600963914, 1.000000000000000000),
 ( 1.000000000000000000, 0.7117460025832214043, 1.000000000000000000),
 ( 1.000000000000000000, 0.7070717283367429218, 1.000000000000000000),
 ( 1.000000000000000000, 0.7071067811865474617, 1.000000000000000000) ) ) 
 REPRESENTATION_ITEM ( '' )  SURFACE ( )  );
#14849 = DIRECTION ( 'NONE',  ( -1.000000000000000000, 0.000000000000000000, -0.000000000000000000 ) ) ;
#14850 = CARTESIAN_POINT ( 'NONE',  ( 0.000000000000000000, 32.49999999999998579, -40.00000000000000000 ) ) ;
#14851 = VECTOR ( 'NONE', #1396, 1000.000000000000000 ) ;
#14852 = CARTESIAN_POINT ( 'NONE',  ( -15.40903463028480580, 38.25937500034140015, 47.42413220539094709 ) ) ;
#14853 = CARTESIAN_POINT ( 'NONE',  ( 49.86468353125001585, 48.75937500034140015, 16.20201782572375038 ) ) ;
#14854 = CARTESIAN_POINT ( 'NONE',  ( -50.00000000000000000, 30.00000000000000355, 0.000000000000000000 ) ) ;
#14855 = DIRECTION ( 'NONE',  ( -0.8660254037844433705, 0.4999999999999918399, 0.000000000000000000 ) ) ;
#14856 = SURFACE_STYLE_FILL_AREA ( #4828 ) ;
#14857 = DIRECTION ( 'NONE',  ( 1.000000000000000000, 0.000000000000000000, 0.000000000000000000 ) ) ;
#14858 = DIRECTION ( 'NONE',  ( 0.000000000000000000, 0.000000000000000000, 1.000000000000000000 ) ) ;
#14859 = CARTESIAN_POINT ( 'NONE',  ( -49.99999999999999289, 33.89999999999999147, -16.24598481164531449 ) ) ;
#14860 = ORIENTED_EDGE ( 'NONE', *, *, #10152, .F. ) ;
#14861 = CARTESIAN_POINT ( 'NONE',  ( -30.81806926056962226, 22.15937500034139873, 42.41743335407647919 ) ) ;
#14862 = ORIENTED_EDGE ( 'NONE', *, *, #7428, .T. ) ;
#14863 = ORIENTED_EDGE ( 'NONE', *, *, #14653, .F. ) ;
#14864 = EDGE_CURVE ( 'NONE', #13242, #13843, #14026, .T. ) ;
#14865 = ADVANCED_FACE ( 'NONE', ( #713 ), #5797, .F. ) ;
#14866 = CARTESIAN_POINT ( 'NONE',  ( 50.00000000000000711, 42.68125000068280173, 16.24598481164530739 ) ) ;
#14867 = DIRECTION ( 'NONE',  ( 0.000000000000000000, 0.000000000000000000, 1.000000000000000000 ) ) ;
#14868 = SURFACE_STYLE_USAGE ( .BOTH. , #6084 ) ;
#14869 = ORIENTED_EDGE ( 'NONE', *, *, #6070, .F. ) ;
#14870 = CARTESIAN_POINT ( 'NONE',  ( -40.45084971874737079, 47.98125000068279888, 29.38926261462367151 ) ) ;
#14871 = CARTESIAN_POINT ( 'NONE',  ( 4.678013043399448456, 44.50832101651065642, 101.0000000000000000 ) ) ;
#14872 = CARTESIAN_POINT ( 'NONE',  ( -17.47218334215669344, 21.35978834315422503, 94.63430745020650647 ) ) ;
#14873 = CARTESIAN_POINT ( 'NONE',  ( -30.00000000000000711, 282.0000000000000000, 12.50000000000000000 ) ) ;
#14874 = DIRECTION ( 'NONE',  ( -0.000000000000000000, -1.000000000000000000, -0.000000000000000000 ) ) ;
#14875 = DIRECTION ( 'NONE',  ( 0.5877852522924797984, -0.8090169943749426773, 0.000000000000000000 ) ) ;
#14876 = CARTESIAN_POINT ( 'NONE',  ( -40.45084971874737789, 47.80000000000000426, -29.38926261462365730 ) ) ;
#14877 = CARTESIAN_POINT ( 'NONE',  ( 5.000000000000000000, 0.000000000000000000, 0.000000000000000000 ) ) ;
#14878 = CARTESIAN_POINT ( 'NONE',  ( -46.00435827497687313, 20.00000000000000355, 19.23833313609354434 ) ) ;
#14879 = CARTESIAN_POINT ( 'NONE',  ( -15.45084971874736368, 44.18125000068280173, 47.55282581475768211 ) ) ;
#14880 = FACE_OUTER_BOUND ( 'NONE', #14374, .T. ) ;
#14881 = CARTESIAN_POINT ( 'NONE',  ( 30.90169943749475578, 30.70000000000000284, 42.53254041760200010 ) ) ;
#14882 = CARTESIAN_POINT ( 'NONE',  ( -40.34137639590981905, 21.65937500034139518, -29.30972558990011478 ) ) ;
#14883 = CARTESIAN_POINT ( 'NONE',  ( -40.45084971874737789, 41.58125000068280031, -29.38926261462365730 ) ) ;
#14884 = ADVANCED_FACE ( 'NONE', ( #15931 ), #4635, .F. ) ;
#14885 = DIRECTION ( 'NONE',  ( -0.000000000000000000, 1.000000000000000000, -0.000000000000000000 ) ) ;
#14886 = EDGE_CURVE ( 'NONE', #12470, #8883, #2043, .T. ) ;
#14887 = ORIENTED_EDGE ( 'NONE', *, *, #564, .F. ) ;
#14888 = DIRECTION ( 'NONE',  ( -0.000000000000000000, -1.000000000000000000, -0.000000000000000000 ) ) ;
#14889 = ORIENTED_EDGE ( 'NONE', *, *, #14545, .F. ) ;
#14890 = CARTESIAN_POINT ( 'NONE',  ( 1.022488062601840571E-14, 49.50000000000000711, -50.00000000000000000 ) ) ;
#14891 = CARTESIAN_POINT ( 'NONE',  ( -30.81806926056963292, 35.55937500034139020, -42.41743335407647209 ) ) ;
#14892 = EDGE_CURVE ( 'NONE', #12041, #5661, #792, .T. ) ;
#14893 = DIRECTION ( 'NONE',  ( -0.5877852522924797984, 0.8090169943749424553, 0.000000000000000000 ) ) ;
#14894 = CARTESIAN_POINT ( 'NONE',  ( 0.000000000000000000, 22.50000000000000000, 101.0000000000000000 ) ) ;
#14895 = CARTESIAN_POINT ( 'NONE',  ( 50.00000000000000000, 28.78125000068279959, -6.123233995736766085E-15 ) ) ;
#14896 = CARTESIAN_POINT ( 'NONE',  ( 0.000000000000000000, 267.0000000000000000, 0.000000000000000000 ) ) ;
#14897 = CARTESIAN_POINT ( 'NONE',  ( 9.631387414534489405E-15, 24.42187500034139447, 52.43083105670540789 ) ) ;
#14898 = CARTESIAN_POINT ( 'NONE',  ( 9.631387414534489405E-15, 30.35937500034139092, 52.43083105670540789 ) ) ;
#14899 = CARTESIAN_POINT ( 'NONE',  ( -30.90169943749474513, 35.69999999999999574, -42.53254041760200721 ) ) ;
#14900 = CARTESIAN_POINT ( 'NONE',  ( -30.81806926056962226, 34.22187500034139163, 42.41743335407647209 ) ) ;
#14901 = PLANE ( 'NONE',  #10787 ) ;
#14902 = CARTESIAN_POINT ( 'NONE',  ( 49.86468353125000164, 46.85937500034139447, -6.106662507704105588E-15 ) ) ;
#14903 = CARTESIAN_POINT ( 'NONE',  ( 49.86468353125000164, 36.92187500034140157, -6.106662507704105588E-15 ) ) ;
#14904 = CARTESIAN_POINT ( 'NONE',  ( 9.657523855033129090E-15, 44.50000000000000711, 52.57311121191334990 ) ) ;
#14905 = VERTEX_POINT ( 'NONE', #14837 ) ;
#14906 = CARTESIAN_POINT ( 'NONE',  ( 30.81806926056964002, 44.55937500034139020, 42.41743335407646498 ) ) ;
#14907 = ORIENTED_EDGE ( 'NONE', *, *, #1297, .F. ) ;
#14908 = CARTESIAN_POINT ( 'NONE',  ( 40.45084971874737079, 24.98125000068279888, -29.38926261462366440 ) ) ;
#14909 = VERTEX_POINT ( 'NONE', #13675 ) ;
#14910 = LINE ( 'NONE', #12343, #11047 ) ;
#14911 = CARTESIAN_POINT ( 'NONE',  ( -49.86468353124999453, 47.82187500034140015, -16.20201782572375393 ) ) ;
#14912 =( REPRESENTATION_RELATIONSHIP ('NONE','NONE', #6178, #9477 ) REPRESENTATION_RELATIONSHIP_WITH_TRANSFORMATION ( #4384 )SHAPE_REPRESENTATION_RELATIONSHIP( ) );
#14913 = CYLINDRICAL_SURFACE ( 'NONE', #6258, 50.00000000000000000 ) ;
#14914 = CARTESIAN_POINT ( 'NONE',  ( -15.40903463028480580, 24.32187500034139660, 47.42413220539094709 ) ) ;
#14915 = CARTESIAN_POINT ( 'NONE',  ( -50.00000000000000000, 35.78125000068280315, 0.000000000000000000 ) ) ;
#14916 = CARTESIAN_POINT ( 'NONE',  ( 30.81806926056964002, 38.62187500034139731, 42.41743335407647209 ) ) ;
#14917 = CARTESIAN_POINT ( 'NONE',  ( 6.123233995736766085E-15, 193.4213562373095385, 50.00000000000000000 ) ) ;
#14918 = ORIENTED_EDGE ( 'NONE', *, *, #14622, .T. ) ;
#14919 = CARTESIAN_POINT ( 'NONE',  ( 15.40903463028481113, 35.32187500034139305, -47.42413220539094709 ) ) ;
#14920 = CARTESIAN_POINT ( 'NONE',  ( -40.45084971874737079, 31.98125000068280244, 29.38926261462367151 ) ) ;
#14921 = ORIENTED_EDGE ( 'NONE', *, *, #13728, .F. ) ;
#14922 = VERTEX_POINT ( 'NONE', #9700 ) ;
#14923 = EDGE_CURVE ( 'NONE', #14296, #1767, #2118, .T. ) ;
#14924 = AXIS2_PLACEMENT_3D ( 'NONE', #10552, #15608, #4230 ) ;
#14925 = ORIENTED_EDGE ( 'NONE', *, *, #12723, .T. ) ;
#14926 = PLANE ( 'NONE',  #4730 ) ;
#14927 = FACE_OUTER_BOUND ( 'NONE', #14533, .T. ) ;
#14928 = CARTESIAN_POINT ( 'NONE',  ( -49.99999999999999289, 49.68125000068279462, -16.24598481164531449 ) ) ;
#14929 = LINE ( 'NONE', #2462, #3685 ) ;
#14930 = CARTESIAN_POINT ( 'NONE',  ( -49.86468353125000164, 39.85937500034139447, 0.000000000000000000 ) ) ;
#14931 = CARTESIAN_POINT ( 'NONE',  ( -30.81806926056962226, 42.15937500034139163, 42.41743335407647209 ) ) ;
#14932 = CARTESIAN_POINT ( 'NONE',  ( 40.45084971874737079, 25.19999999999999929, -29.38926261462366440 ) ) ;
#14933 = EDGE_CURVE ( 'NONE', #15902, #15466, #4978, .T. ) ;
#14934 = EDGE_CURVE ( 'NONE', #7759, #16058, #15090, .T. ) ;
#14935 = DIRECTION ( 'NONE',  ( 0.000000000000000000, 0.000000000000000000, 1.000000000000000000 ) ) ;
#14936 =( LENGTH_UNIT ( ) NAMED_UNIT ( * ) SI_UNIT ( .MILLI., .METRE. ) );
#14937 = CARTESIAN_POINT ( 'NONE',  ( -48.35726954556750457, 20.00000000000000355, 12.16803787670978387 ) ) ;
#14938 = CIRCLE ( 'NONE', #6747, 10.00000000000000355 ) ;
#14939 = CARTESIAN_POINT ( 'NONE',  ( -1.240322475938754499E-13, 40.50000000000000000, 50.00000000000000000 ) ) ;
#14940 = ADVANCED_FACE ( 'NONE', ( #16184 ), #1603, .T. ) ;
#14941 = CARTESIAN_POINT ( 'NONE',  ( 5.755839955992560641E-15, 25.00000000000000000, 47.00000000000000000 ) ) ;
#14942 = VERTEX_POINT ( 'NONE', #511 ) ;
#14943 = CARTESIAN_POINT ( 'NONE',  ( -40.34137639590981905, 21.65937500034139518, -29.30972558990011478 ) ) ;
#14944 = LINE ( 'NONE', #13803, #2277 ) ;
#14945 = ORIENTED_EDGE ( 'NONE', *, *, #10387, .F. ) ;
#14946 = ORIENTED_EDGE ( 'NONE', *, *, #15358, .T. ) ;
#14947 =( BOUNDED_CURVE ( )  B_SPLINE_CURVE ( 2, ( #425, #3092, #9168, #8170, #4193, #7835, #8078, #1597, #10744, #5530, #10591, #4271, #13238 ),
 .UNSPECIFIED., .F., .T. ) 
 B_SPLINE_CURVE_WITH_KNOTS ( ( 3, 2, 2, 2, 2, 2, 3 ),
 ( 0.9166666666666667407, 0.9200000000000000400, 0.9266666666666666385, 0.9333333333333333481, 0.9399999999999999467, 0.9466666666666666563, 0.9500000000000000666 ),
 .UNSPECIFIED. ) 
 CURVE ( )  GEOMETRIC_REPRESENTATION_ITEM ( )  RATIONAL_B_SPLINE_CURVE ( ( 0.9755282581475768211, 0.9755282581475771542, 1.000000000000000000, 0.9510565162951535312, 1.000000000000000000, 0.9510565162951535312, 1.000000000000000000, 0.9510565162951535312, 1.000000000000000000, 0.9510565162951535312, 1.000000000000000000, 0.9755282581475763770, 0.9755282581475768211 ) ) 
 REPRESENTATION_ITEM ( '' )  );
#14948 = CARTESIAN_POINT ( 'NONE',  ( 30.90169943749474157, 41.08125000068280031, -42.53254041760200721 ) ) ;
#14949 = CARTESIAN_POINT ( 'NONE',  ( -15.45084971874736368, 40.40000000000000568, 47.55282581475768211 ) ) ;
#14950 = DIRECTION ( 'NONE',  ( 0.000000000000000000, -1.000000000000000000, 0.000000000000000000 ) ) ;
#14952 = ORIENTED_EDGE ( 'NONE', *, *, #210, .T. ) ;
#14951 = AXIS2_PLACEMENT_3D ( 'NONE', #829, #749, #16138 ) ;
#14953 = CARTESIAN_POINT ( 'NONE',  ( 9.297345850538470396E-15, 92.00000000000001421, -1.969248798088869855E-14 ) ) ;
#14954 =( NAMED_UNIT ( * ) SI_UNIT ( $, .STERADIAN. ) SOLID_ANGLE_UNIT ( ) );
#14955 = CARTESIAN_POINT ( 'NONE',  ( -3.149380788943775933, 5.278461141749506425, 101.0000000000000000 ) ) ;
#14956 = CARTESIAN_POINT ( 'NONE',  ( 0.000000000000000000, 52.00000000000000711, 0.000000000000000000 ) ) ;
#14957 = CARTESIAN_POINT ( 'NONE',  ( 5.000000000000000000, 96.75198296766784267, -7.580410092414001433 ) ) ;
#14958 = DIRECTION ( 'NONE',  ( -0.000000000000000000, 1.000000000000000000, -0.000000000000000000 ) ) ;
#14959 = CARTESIAN_POINT ( 'NONE',  ( 0.5000000000000001110, 39.32590460608501104, 101.6666710454654208 ) ) ;
#14960 = CARTESIAN_POINT ( 'NONE',  ( -24.14213562373095101, 282.0000000000000000, -9.571067811865473729 ) ) ;
#14961 = CARTESIAN_POINT ( 'NONE',  ( -45.67643563157982101, 19.99999999999998934, 20.00444126042745197 ) ) ;
#14962 = CARTESIAN_POINT ( 'NONE',  ( 49.99999999999999289, 46.88125000068279036, -16.24598481164532160 ) ) ;
#14963 = CARTESIAN_POINT ( 'NONE',  ( 6.658212670116058440, 38.68388717334331517, 101.0000000000000000 ) ) ;
#14964 = CARTESIAN_POINT ( 'NONE',  ( -49.99999999999999289, 29.89999999999999858, -16.24598481164531449 ) ) ;
#14965 = CARTESIAN_POINT ( 'NONE',  ( 5.755839955992560641E-15, 193.4213562373095385, 47.00000000000000000 ) ) ;
#14966 = DIRECTION ( 'NONE',  ( 0.000000000000000000, 0.000000000000000000, 1.000000000000000000 ) ) ;
#14967 = CIRCLE ( 'NONE', #1711, 47.00000000000000000 ) ;
#14968 = CARTESIAN_POINT ( 'NONE',  ( 49.86468353125001585, 42.75937500034138594, 16.20201782572375038 ) ) ;
#14969 = ORIENTED_EDGE ( 'NONE', *, *, #4986, .F. ) ;
#14970 = LINE ( 'NONE', #12157, #3859 ) ;
#14971 = ORIENTED_EDGE ( 'NONE', *, *, #5117, .T. ) ;
#14972 = DIRECTION ( 'NONE',  ( 0.000000000000000000, 0.000000000000000000, 1.000000000000000000 ) ) ;
#14973 = CARTESIAN_POINT ( 'NONE',  ( -40.34137639590981905, 35.65937500034139873, -29.30972558990011478 ) ) ;
#14974 = FACE_OUTER_BOUND ( 'NONE', #10868, .T. ) ;
#14975 = FACE_OUTER_BOUND ( 'NONE', #11730, .T. ) ;
#14976 = CARTESIAN_POINT ( 'NONE',  ( -37.77664397204053159, 40.00000000000000711, -13.15010152849376190 ) ) ;
#14977 = AXIS2_PLACEMENT_3D ( 'NONE', #1984, #11593, #15411 ) ;
#14978 = CYLINDRICAL_SURFACE ( 'NONE', #4701, 50.00000000000000000 ) ;
#14979 = CARTESIAN_POINT ( 'NONE',  ( 9.631387414534489405E-15, 20.42187500034139802, 52.43083105670540789 ) ) ;
#14980 = CARTESIAN_POINT ( 'NONE',  ( -15.40903463028480580, 28.25937500034139660, 47.42413220539094709 ) ) ;
#14981 = DIRECTION ( 'NONE',  ( -0.9135454576426060846, 0.4067366430757887730, 0.000000000000000000 ) ) ;
#14982 = CARTESIAN_POINT ( 'NONE',  ( 40.34137639590981905, 32.72187500034139873, 29.30972558990010768 ) ) ;
#14983 = DIRECTION ( 'NONE',  ( 1.000000000000000000, 0.000000000000000000, 0.000000000000000000 ) ) ;
#14984 = CARTESIAN_POINT ( 'NONE',  ( 15.40903463028482356, 36.45937500034139589, 47.42413220539093999 ) ) ;
#14985 = CARTESIAN_POINT ( 'NONE',  ( -30.81806926056962226, 38.22187500034139873, 42.41743335407647919 ) ) ;
#14986 = CARTESIAN_POINT ( 'NONE',  ( -3.219174618344376363E-15, 47.49999999999999289, -52.57311121191334990 ) ) ;
#14987 = EDGE_CURVE ( 'NONE', #4733, #15952, #2032, .T. ) ;
#14988 = EDGE_LOOP ( 'NONE', ( #2342, #5639, #5680, #1821, #250, #3198 ) ) ;
#14989 = VECTOR ( 'NONE', #14052, 1000.000000000000000 ) ;
#14990 = CARTESIAN_POINT ( 'NONE',  ( -49.86468353124999453, 45.75937500034140015, -16.20201782572375393 ) ) ;
#14991 = ORIENTED_EDGE ( 'NONE', *, *, #11036, .T. ) ;
#14992 = CARTESIAN_POINT ( 'NONE',  ( -40.45084971874737079, 23.98125000068279888, 29.38926261462367151 ) ) ;
#14993 = CARTESIAN_POINT ( 'NONE',  ( -2.547328955960238000E-13, 34.50000000000000000, 49.99999999999999289 ) ) ;
#14994 = CARTESIAN_POINT ( 'NONE',  ( 15.45084971874737789, 40.38125000068280457, 47.55282581475767500 ) ) ;
#14995 = CARTESIAN_POINT ( 'NONE',  ( 49.86468353124999453, 41.02187500034139589, -16.20201782572376459 ) ) ;
#14996 = CARTESIAN_POINT ( 'NONE',  ( 15.45084971874737789, 40.60000000000000142, 47.55282581475767500 ) ) ;
#14997 = CIRCLE ( 'NONE', #11299, 87.81953344283027718 ) ;
#14998 = CARTESIAN_POINT ( 'NONE',  ( 49.86468353125001585, 26.82187500034138949, 16.20201782572375038 ) ) ;
#14999 = CARTESIAN_POINT ( 'NONE',  ( 40.45084971874737079, 28.98125000068279888, -29.38926261462366440 ) ) ;
#15000 = PRESENTATION_LAYER_ASSIGNMENT (  '', '', ( #7583 ) ) ;
#15001 = CARTESIAN_POINT ( 'NONE',  ( 30.81806926056964002, 32.62187500034140442, 42.41743335407647209 ) ) ;
#15002 = CARTESIAN_POINT ( 'NONE',  ( -22.04892374372078834, 283.9500510409131948, -8.524461871855592676 ) ) ;
#15003 = CARTESIAN_POINT ( 'NONE',  ( -15.40903463028480580, 36.32187500034140015, 47.42413220539094709 ) ) ;
#15004 = CARTESIAN_POINT ( 'NONE',  ( -50.00000000000000000, 41.78125000068280315, 0.000000000000000000 ) ) ;
#15005 = ORIENTED_EDGE ( 'NONE', *, *, #6524, .F. ) ;
#15006 = AXIS2_PLACEMENT_3D ( 'NONE', #3285, #16175, #4805 ) ;
#15007 = VERTEX_POINT ( 'NONE', #6382 ) ;
#15008 = CONICAL_SURFACE ( 'NONE', #9188, 49.99999999999999289, 0.7853981633974642662 ) ;
#15009 = ORIENTED_EDGE ( 'NONE', *, *, #11413, .T. ) ;
#15010 = CYLINDRICAL_SURFACE ( 'NONE', #10561, 5.000000000000000000 ) ;
#15011 = CARTESIAN_POINT ( 'NONE',  ( -5.000000000000000000, 121.6750890729883565, 29.67508907298824283 ) ) ;
#15012 = EDGE_CURVE ( 'NONE', #1326, #15748, #2855, .T. ) ;
#15013 = LINE ( 'NONE', #2054, #9454 ) ;
#15014 = PLANE ( 'NONE',  #2617 ) ;
#15015 = CARTESIAN_POINT ( 'NONE',  ( -49.86468353125000164, 29.85937500034139802, 0.000000000000000000 ) ) ;
#15016 = CARTESIAN_POINT ( 'NONE',  ( 15.40903463028482356, 40.45937500034139589, 47.42413220539093999 ) ) ;
#15017 =( LENGTH_UNIT ( ) NAMED_UNIT ( * ) SI_UNIT ( .MILLI., .METRE. ) );
#15018 = DIRECTION ( 'NONE',  ( -1.000000000000000000, 0.000000000000000000, 0.000000000000000000 ) ) ;
#15019 = AXIS2_PLACEMENT_3D ( 'NONE', #8043, #13114, #1720 ) ;
#15020 = AXIS2_PLACEMENT_3D ( 'NONE', #7995, #8073, #1755 ) ;
#15022 = DIRECTION ( 'NONE',  ( -1.000000000000000000, 0.000000000000000000, 0.000000000000000000 ) ) ;
#15021 = AXIS2_PLACEMENT_3D ( 'NONE', #11067, #14788, #9981 ) ;
#15023 = VECTOR ( 'NONE', #1398, 1000.000000000000000 ) ;
#15024 = CARTESIAN_POINT ( 'NONE',  ( 0.000000000000000000, 193.4213562373095385, 0.000000000000000000 ) ) ;
#15025 = DIRECTION ( 'NONE',  ( 0.000000000000000000, 1.000000000000000000, 0.000000000000000000 ) ) ;
#15026 = VERTEX_POINT ( 'NONE', #37 ) ;
#15027 = CARTESIAN_POINT ( 'NONE',  ( 40.34137639590981195, 25.05937500034139376, -29.30972558990011834 ) ) ;
#15028 = VERTEX_POINT ( 'NONE', #8861 ) ;
#15029 = EDGE_CURVE ( 'NONE', #7317, #13034, #6779, .T. ) ;
#15030 = ORIENTED_EDGE ( 'NONE', *, *, #10990, .T. ) ;
#15031 = ORIENTED_EDGE ( 'NONE', *, *, #11703, .F. ) ;
#15032 = CARTESIAN_POINT ( 'NONE',  ( 30.90169943749474157, 35.08125000068278609, -42.53254041760200721 ) ) ;
#15033 = AXIS2_PLACEMENT_3D ( 'NONE', #12283, #5896, #3483 ) ;
#15034 = LINE ( 'NONE', #9976, #6566 ) ;
#15035 = CARTESIAN_POINT ( 'NONE',  ( 0.000000000000000000, 272.0000000000000000, -79.49773270518484480 ) ) ;
#15036 = VECTOR ( 'NONE', #10084, 1000.000000000000227 ) ;
#15037 = ORIENTED_EDGE ( 'NONE', *, *, #1049, .F. ) ;
#15038 = PLANE ( 'NONE',  #8885 ) ;
#15039 = DIRECTION ( 'NONE',  ( 1.000000000000000000, 0.000000000000000000, 0.000000000000000000 ) ) ;
#15040 = EDGE_CURVE ( 'NONE', #12589, #11148, #11823, .T. ) ;
#15041 = CARTESIAN_POINT ( 'NONE',  ( 2.499999999999999556, 247.0000000000000568, 49.17157287525380127 ) ) ;
#15042 = CYLINDRICAL_SURFACE ( 'NONE', #5427, 82.49773270518484480 ) ;
#15043 = CYLINDRICAL_SURFACE ( 'NONE', #492, 10.00000000000000355 ) ;
#15044 = CARTESIAN_POINT ( 'NONE',  ( -5.000000000000000000, 90.58578643762692195, 1.414213562373097588 ) ) ;
#15045 = FACE_OUTER_BOUND ( 'NONE', #13763, .T. ) ;
#15046 = CARTESIAN_POINT ( 'NONE',  ( -50.00000000000000000, 49.78125000068280315, 0.000000000000000000 ) ) ;
#15047 = CARTESIAN_POINT ( 'NONE',  ( 15.45084971874736723, 21.40000000000000213, -47.55282581475768211 ) ) ;
#15048 = EDGE_CURVE ( 'NONE', #758, #10725, #8174, .T. ) ;
#15049 = CARTESIAN_POINT ( 'NONE',  ( 49.99999999999999289, 31.09999999999999787, -16.24598481164532160 ) ) ;
#15050 = CARTESIAN_POINT ( 'NONE',  ( -49.86468353125000164, 21.85937500034139802, 0.000000000000000000 ) ) ;
#15051 = VECTOR ( 'NONE', #7695, 1000.000000000000000 ) ;
#15052 = DIRECTION ( 'NONE',  ( 1.000000000000000000, 0.000000000000000000, 0.000000000000000000 ) ) ;
#15054 =( BOUNDED_CURVE ( )  B_SPLINE_CURVE ( 2, ( #13188, #8199, #7952, #9534, #1707, #10449, #1626, #13265, #15751, #1792, #4467, #14578, #6720 ),
 .UNSPECIFIED., .F., .T. ) 
 B_SPLINE_CURVE_WITH_KNOTS ( ( 3, 2, 2, 2, 2, 2, 3 ),
 ( 0.5500000000000000444, 0.5533333333333333437, 0.5600000000000000533, 0.5666666666666666519, 0.5733333333333333615, 0.5799999999999999600, 0.5833333333333333703 ),
 .UNSPECIFIED. ) 
 CURVE ( )  GEOMETRIC_REPRESENTATION_ITEM ( )  RATIONAL_B_SPLINE_CURVE ( ( 0.9755282581475768211, 0.9755282581475771542, 1.000000000000000000, 0.9510565162951535312, 1.000000000000000000, 0.9510565162951535312, 1.000000000000000000, 0.9510565162951535312, 1.000000000000000000, 0.9510565162951535312, 1.000000000000000000, 0.9755282581475763770, 0.9755282581475768211 ) ) 
 REPRESENTATION_ITEM ( '' )  );
#15053 = VECTOR ( 'NONE', #15688, 1000.000000000000000 ) ;
#15055 = CARTESIAN_POINT ( 'NONE',  ( 30.81806926056964002, 42.55937500034139020, 42.41743335407647209 ) ) ;
#15056 = EDGE_LOOP ( 'NONE', ( #2048, #1386, #3738 ) ) ;
#15057 = SURFACE_SIDE_STYLE ('',( #7820 ) ) ;
#15058 = ORIENTED_EDGE ( 'NONE', *, *, #13348, .T. ) ;
#15059 = DIRECTION ( 'NONE',  ( 0.000000000000000000, -1.000000000000000000, 0.000000000000000000 ) ) ;
#15060 = CARTESIAN_POINT ( 'NONE',  ( 40.34137639590981195, 37.05937500034139731, -29.30972558990011834 ) ) ;
#15061 = ADVANCED_FACE ( 'NONE', ( #1601 ), #6695, .T. ) ;
#15062 = CARTESIAN_POINT ( 'NONE',  ( 0.000000000000000000, 262.0000000000000000, 0.000000000000000000 ) ) ;
#15063 = CARTESIAN_POINT ( 'NONE',  ( 0.000000000000000000, 52.00000000000000711, 63.16733765196516970 ) ) ;
#15064 = CARTESIAN_POINT ( 'NONE',  ( 46.85365039762147177, 25.00000000000000711, -17.06523097087115914 ) ) ;
#15065 = DIRECTION ( 'NONE',  ( 0.000000000000000000, 0.000000000000000000, 1.000000000000000000 ) ) ;
#15066 = CARTESIAN_POINT ( 'NONE',  ( -15.40903463028481646, 23.52187500034139944, -47.42413220539093999 ) ) ;
#15067 = CARTESIAN_POINT ( 'NONE',  ( 30.81806926056964002, 20.55937500034139376, 42.41743335407646498 ) ) ;
#15068 = DIRECTION ( 'NONE',  ( 0.9781476007338042455, 0.2079116908177664758, 0.000000000000000000 ) ) ;
#15069 = CARTESIAN_POINT ( 'NONE',  ( -3.210462471511496205E-15, 33.42187500034139447, -52.43083105670540789 ) ) ;
#15070 = CARTESIAN_POINT ( 'NONE',  ( -15.45084971874737256, 29.38125000068279746, -47.55282581475767500 ) ) ;
#15071 = CARTESIAN_POINT ( 'NONE',  ( -30.90169943749473802, 40.30000000000000426, 42.53254041760200721 ) ) ;
#15072 = CARTESIAN_POINT ( 'NONE',  ( -49.86468353124999453, 39.75937500034139305, -16.20201782572375393 ) ) ;
#15073 = CARTESIAN_POINT ( 'NONE',  ( -15.40903463028481646, 33.52187500034140299, -47.42413220539093999 ) ) ;
#15074 = CARTESIAN_POINT ( 'NONE',  ( 30.90169943749475578, 46.69999999999999574, 42.53254041760200010 ) ) ;
#15075 = EDGE_LOOP ( 'NONE', ( #9405, #7229, #15745, #7966 ) ) ;
#15076 = CARTESIAN_POINT ( 'NONE',  ( 9.631387414534489405E-15, 38.35937500034139447, 52.43083105670540789 ) ) ;
#15077 = EDGE_LOOP ( 'NONE', ( #7844, #16039, #6013, #814 ) ) ;
#15078 = EDGE_LOOP ( 'NONE', ( #1920, #11723, #12385, #8021 ) ) ;
#15079 = EDGE_CURVE ( 'NONE', #9091, #5374, #5445, .T. ) ;
#15080 = CARTESIAN_POINT ( 'NONE',  ( 40.45084971874737789, 24.58125000068280031, 29.38926261462365375 ) ) ;
#15081 = DIRECTION ( 'NONE',  ( 0.000000000000000000, -0.000000000000000000, -1.000000000000000000 ) ) ;
#15082 = CARTESIAN_POINT ( 'NONE',  ( -40.34137639590981905, 23.72187500034139873, -29.30972558990011478 ) ) ;
#15083 = CARTESIAN_POINT ( 'NONE',  ( 0.000000000000000000, 262.0000000000000000, 0.000000000000000000 ) ) ;
#15084 = CIRCLE ( 'NONE', #10324, 50.00000000000000000 ) ;
#15085 = CARTESIAN_POINT ( 'NONE',  ( 49.86468353125000164, 42.92187500034140157, -6.106662507704105588E-15 ) ) ;
#15086 = CARTESIAN_POINT ( 'NONE',  ( 8.446640517145639571E-15, 26.28125000068279959, 50.00000000000000000 ) ) ;
#15087 = CARTESIAN_POINT ( 'NONE',  ( -40.45084971874737789, 49.80000000000000426, -29.38926261462365730 ) ) ;
#15088 = CARTESIAN_POINT ( 'NONE',  ( -40.45084971874737789, 29.58125000068279675, -29.38926261462365730 ) ) ;
#15089 = CARTESIAN_POINT ( 'NONE',  ( 30.81806926056964002, 36.62187500034139731, 42.41743335407647209 ) ) ;
#15090 = LINE ( 'NONE', #3467, #1666 ) ;
#15091 = CARTESIAN_POINT ( 'NONE',  ( -30.81806926056962226, 36.22187500034139873, 42.41743335407647919 ) ) ;
#15092 = AXIS2_PLACEMENT_3D ( 'NONE', #7484, #10315, #14117 ) ;
#15093 = CARTESIAN_POINT ( 'NONE',  ( -49.99999999999999289, 31.68125000068279462, -16.24598481164531449 ) ) ;
#15094 = EDGE_LOOP ( 'NONE', ( #323, #941, #1276, #9727 ) ) ;
#15095 = SHAPE_REPRESENTATION ( 'rubber clutch', ( #15812 ), #10512 ) ;
#15096 = ORIENTED_EDGE ( 'NONE', *, *, #7708, .T. ) ;
#15097 = CARTESIAN_POINT ( 'NONE',  ( -5.000000000000000000, 0.000000000000000000, 0.000000000000000000 ) ) ;
#15098 = CARTESIAN_POINT ( 'NONE',  ( -3.111920190527341144E-15, 45.50000000000000000, -50.00000000000000000 ) ) ;
#15099 = CARTESIAN_POINT ( 'NONE',  ( 10.69075041230586365, 8.636095224584757091, 101.0000000000000000 ) ) ;
#15100 = DIRECTION ( 'NONE',  ( 0.1045284632676570929, -0.9945218953682730678, 0.000000000000000000 ) ) ;
#15101 = CARTESIAN_POINT ( 'NONE',  ( 15.40903463028481113, 29.25937500034139660, -47.42413220539094709 ) ) ;
#15102 =( NAMED_UNIT ( * ) PLANE_ANGLE_UNIT ( ) SI_UNIT ( $, .RADIAN. ) );
#15103 = CARTESIAN_POINT ( 'NONE',  ( 30.81806926056964002, 44.62187500034139731, 42.41743335407646498 ) ) ;
#15104 =( NAMED_UNIT ( * ) PLANE_ANGLE_UNIT ( ) SI_UNIT ( $, .RADIAN. ) );
#15105 = CARTESIAN_POINT ( 'NONE',  ( -3.111920190527341144E-15, 35.28125000068280315, -50.00000000000000000 ) ) ;
#15106 = CARTESIAN_POINT ( 'NONE',  ( 2.500000000000000000, 247.0000000000000284, -40.00000000000000000 ) ) ;
#15107 = FACE_OUTER_BOUND ( 'NONE', #12026, .T. ) ;
#15108 = ORIENTED_EDGE ( 'NONE', *, *, #9318, .F. ) ;
#15109 = CARTESIAN_POINT ( 'NONE',  ( -49.86468353125000164, 23.85937500034139447, 0.000000000000000000 ) ) ;
#15110 = ORIENTED_EDGE ( 'NONE', *, *, #5307, .F. ) ;
#15111 = CARTESIAN_POINT ( 'NONE',  ( -7.919222016226802552, 47.33250428222964956, -50.00000000000000000 ) ) ;
#15112 = ORIENTED_EDGE ( 'NONE', *, *, #13914, .F. ) ;
#15113 = ORIENTED_EDGE ( 'NONE', *, *, #4920, .F. ) ;
#15114 = CARTESIAN_POINT ( 'NONE',  ( 0.000000000000000000, 262.0000000000000000, 0.000000000000000000 ) ) ;
#15115 = PLANE ( 'NONE',  #9424 ) ;
#15116 = VERTEX_POINT ( 'NONE', #2538 ) ;
#15117 = CARTESIAN_POINT ( 'NONE',  ( 8.477241335952196977, 18.18301270189230578, 101.0000000000000000 ) ) ;
#15118 = CARTESIAN_POINT ( 'NONE',  ( -40.45084971874737789, 37.79999999999999716, -29.38926261462365730 ) ) ;
#15119 = CARTESIAN_POINT ( 'NONE',  ( 9.397478011314830142E-15, 52.00000000000000711, -45.00000000000002842 ) ) ;
#15120 = CARTESIAN_POINT ( 'NONE',  ( 27.07106781186547551, 282.0000000000000000, 6.642135623730952787 ) ) ;
#15121 = CARTESIAN_POINT ( 'NONE',  ( 7.919222016226822092, 26.33250428222964246, 49.99999999999999289 ) ) ;
#15122 = FACE_OUTER_BOUND ( 'NONE', #11461, .T. ) ;
#15123 = CARTESIAN_POINT ( 'NONE',  ( 0.000000000000000000, 51.99999999999999289, 0.000000000000000000 ) ) ;
#15124 = CARTESIAN_POINT ( 'NONE',  ( 10.29452708129665162, 9.181449853854692478, 101.6666710451724214 ) ) ;
#15125 = CARTESIAN_POINT ( 'NONE',  ( -30.90169943749474868, 49.48125000068279178, -42.53254041760200721 ) ) ;
#15126 = CARTESIAN_POINT ( 'NONE',  ( 6.522576737113721101, 38.37924387995723663, 101.3333374614808662 ) ) ;
#15127 = DIRECTION ( 'NONE',  ( -1.000000000000000000, 0.000000000000000000, 0.000000000000000000 ) ) ;
#15128 = CARTESIAN_POINT ( 'NONE',  ( 0.000000000000000000, 50.00000000000000000, -85.01963570546854498 ) ) ;
#15129 = CARTESIAN_POINT ( 'NONE',  ( -2.317185599438165467E-15, 40.00000000000004974, 92.94692077166139654 ) ) ;
#15130 = CARTESIAN_POINT ( 'NONE',  ( 40.34137639590981905, 44.65937500034139163, 29.30972558990010768 ) ) ;
#15131 = ORIENTED_EDGE ( 'NONE', *, *, #15522, .F. ) ;
#15132 = VERTEX_POINT ( 'NONE', #13154 ) ;
#15133 = CARTESIAN_POINT ( 'NONE',  ( 0.000000000000000000, 272.0000000000000000, -42.00000000000000711 ) ) ;
#15134 = CARTESIAN_POINT ( 'NONE',  ( 15.40903463028481113, 29.25937500034139660, -47.42413220539094709 ) ) ;
#15135 = EDGE_CURVE ( 'NONE', #15748, #1641, #10671, .T. ) ;
#15136 = CARTESIAN_POINT ( 'NONE',  ( -33.58330087751660642, 29.97008732934372333, -22.31061932476956855 ) ) ;
#15137 = CARTESIAN_POINT ( 'NONE',  ( -4.545615046168190787, 39.40905366563087853, 92.94163982466287166 ) ) ;
#15138 = CARTESIAN_POINT ( 'NONE',  ( 45.18727525474233175, 25.00000000000000711, -21.08615623785931348 ) ) ;
#15139 = CARTESIAN_POINT ( 'NONE',  ( 49.86468353125001585, 32.82187500034139305, 16.20201782572375038 ) ) ;
#15140 = CARTESIAN_POINT ( 'NONE',  ( 9.297345850538470396E-15, 92.00000000000001421, -1.969248798088869855E-14 ) ) ;
#15141 = CARTESIAN_POINT ( 'NONE',  ( 30.81806926056962936, 25.22187500034139873, -42.41743335407647209 ) ) ;
#15142 = CARTESIAN_POINT ( 'NONE',  ( 15.40903463028481113, 21.25937500034139660, -47.42413220539094709 ) ) ;
#15143 = FACE_OUTER_BOUND ( 'NONE', #3818, .T. ) ;
#15144 = CARTESIAN_POINT ( 'NONE',  ( 9.631387414534489405E-15, 32.42187500034139447, 52.43083105670540789 ) ) ;
#15145 = ADVANCED_FACE ( 'NONE', ( #14316 ), #2935, .T. ) ;
#15146 = CARTESIAN_POINT ( 'NONE',  ( 7.919222016226693306, 32.55125428154685352, 50.00000000000003553 ) ) ;
#15147 = EDGE_CURVE ( 'NONE', #2544, #1479, #674, .T. ) ;
#15148 = CARTESIAN_POINT ( 'NONE',  ( -40.45084971874737079, 34.20000000000000284, 29.38926261462367151 ) ) ;
#15149 = CARTESIAN_POINT ( 'NONE',  ( 15.40903463028482356, 38.45937500034139589, 47.42413220539093999 ) ) ;
#15150 = CARTESIAN_POINT ( 'NONE',  ( 9.631387414534489405E-15, 28.42187500034139092, 52.43083105670540789 ) ) ;
#15151 = ADVANCED_FACE ( 'NONE', ( #3099 ), #8039, .T. ) ;
#15152 = CARTESIAN_POINT ( 'NONE',  ( 49.99999999999999289, 45.10000000000000853, -16.24598481164532160 ) ) ;
#15153 = ORIENTED_EDGE ( 'NONE', *, *, #8026, .F. ) ;
#15154 = CARTESIAN_POINT ( 'NONE',  ( 40.34137639590981905, 38.65937500034139873, 29.30972558990010768 ) ) ;
#15155 = ORIENTED_EDGE ( 'NONE', *, *, #7444, .F. ) ;
#15156 = ORIENTED_EDGE ( 'NONE', *, *, #963, .T. ) ;
#15157 = DIRECTION ( 'NONE',  ( 0.000000000000000000, 0.000000000000000000, -1.000000000000000000 ) ) ;
#15158 = CARTESIAN_POINT ( 'NONE',  ( -30.81806926056962226, 46.15937500034139873, 42.41743335407647919 ) ) ;
#15159 = CARTESIAN_POINT ( 'NONE',  ( 2.600676159226420495E-13, 33.49999999999999289, -49.99999999999999289 ) ) ;
#15160 = CARTESIAN_POINT ( 'NONE',  ( -49.86468353124999453, 22.02187500034139589, 16.20201782572377525 ) ) ;
#15161 = CARTESIAN_POINT ( 'NONE',  ( -3.147895402235901141, 5.285449336779595164, 101.0000000000000000 ) ) ;
#15162 = CARTESIAN_POINT ( 'NONE',  ( 15.40903463028482356, 40.52187500034139589, 47.42413220539093999 ) ) ;
#15163 = CARTESIAN_POINT ( 'NONE',  ( -25.00000000000000355, 287.0000000000000568, -7.499999999999999112 ) ) ;
#15164 = CARTESIAN_POINT ( 'NONE',  ( 40.45084971874737079, 47.20000000000000284, -29.38926261462366440 ) ) ;
#15165 = CARTESIAN_POINT ( 'NONE',  ( -3.219174618344376363E-15, 29.28125000068279604, -52.57311121191334990 ) ) ;
#15166 = CARTESIAN_POINT ( 'NONE',  ( -49.86468353124999453, 48.02187500034139589, 16.20201782572377525 ) ) ;
#15167 = ADVANCED_FACE ( 'NONE', ( #15722 ), #1839, .T. ) ;
#15168 = CARTESIAN_POINT ( 'NONE',  ( -30.81806926056963292, 31.62187500034139731, -42.41743335407647209 ) ) ;
#15169 = CARTESIAN_POINT ( 'NONE',  ( 40.45084971874737079, 39.19999999999999574, -29.38926261462366440 ) ) ;
#15170 = EDGE_CURVE ( 'NONE', #286, #11447, #16148, .T. ) ;
#15171 = DIRECTION ( 'NONE',  ( 0.9961946980917455452, 0.08715574274765824914, 0.000000000000000000 ) ) ;
#15172 = VERTEX_POINT ( 'NONE', #1999 ) ;
#15173 = EDGE_LOOP ( 'NONE', ( #6464, #4007, #10511, #11350 ) ) ;
#15174 = CARTESIAN_POINT ( 'NONE',  ( -20.00000000000000355, 312.0000000000000568, 0.000000000000000000 ) ) ;
#15175 = CARTESIAN_POINT ( 'NONE',  ( 50.00000000000000711, 44.90000000000000568, 16.24598481164530739 ) ) ;
#15176 = CARTESIAN_POINT ( 'NONE',  ( 0.000000000000000000, 28.00000000000000355, -10.00000000000000000 ) ) ;
#15177 = CARTESIAN_POINT ( 'NONE',  ( -49.86468353124999453, 29.95937500034139944, 16.20201782572377525 ) ) ;
#15178 = SURFACE_STYLE_FILL_AREA ( #14016 ) ;
#15179 = CARTESIAN_POINT ( 'NONE',  ( 15.40903463028481113, 47.32187500034140015, -47.42413220539094709 ) ) ;
#15180 = DIRECTION ( 'NONE',  ( 0.000000000000000000, 0.000000000000000000, -1.000000000000000000 ) ) ;
#15181 = LINE ( 'NONE', #3812, #11629 ) ;
#15182 = CARTESIAN_POINT ( 'NONE',  ( -15.45084971874737256, 41.60000000000000142, -47.55282581475767500 ) ) ;
#15183 = VERTEX_POINT ( 'NONE', #12315 ) ;
#15184 = EDGE_CURVE ( 'NONE', #12542, #13034, #13315, .T. ) ;
#15185 = VECTOR ( 'NONE', #8304, 1000.000000000000000 ) ;
#15186 = CARTESIAN_POINT ( 'NONE',  ( -49.86468353124999453, 27.95937500034139944, 16.20201782572377525 ) ) ;
#15187 = EDGE_CURVE ( 'NONE', #8086, #14691, #12023, .T. ) ;
#15188 = ORIENTED_EDGE ( 'NONE', *, *, #8988, .F. ) ;
#15189 = LINE ( 'NONE', #7964, #5495 ) ;
#15190 = VERTEX_POINT ( 'NONE', #9660 ) ;
#15191 = VERTEX_POINT ( 'NONE', #10833 ) ;
#15192 = CARTESIAN_POINT ( 'NONE',  ( -1.240322475938754499E-13, 40.28125000068280315, 50.00000000000000000 ) ) ;
#15193 = DIRECTION ( 'NONE',  ( 1.000000000000000000, 0.000000000000000000, 0.000000000000000000 ) ) ;
#15194 = DIRECTION ( 'NONE',  ( 0.000000000000000000, 0.000000000000000000, 1.000000000000000000 ) ) ;
#15195 = PLANE ( 'NONE',  #11941 ) ;
#15196 = CARTESIAN_POINT ( 'NONE',  ( -8.660254037844415720, 37.00000000000001421, -4.999999999999952038 ) ) ;
#15197 = DIRECTION ( 'NONE',  ( -1.000000000000000000, 0.000000000000000000, 0.000000000000000000 ) ) ;
#15198 = LINE ( 'NONE', #1319, #15898 ) ;
#15199 = AXIS2_PLACEMENT_3D ( 'NONE', #4785, #14639, #5855 ) ;
#15200 = CARTESIAN_POINT ( 'NONE',  ( -43.87482193696061472, 267.0000000000000000, 10.00000000000000178 ) ) ;
#15201 = CARTESIAN_POINT ( 'NONE',  ( 30.90169943749475578, 44.48125000068279888, 42.53254041760200010 ) ) ;
#15202 = CARTESIAN_POINT ( 'NONE',  ( 15.45084971874737789, 44.38125000068279746, 47.55282581475767500 ) ) ;
#15203 = CARTESIAN_POINT ( 'NONE',  ( 30.90169943749475578, 22.69999999999999929, 42.53254041760200010 ) ) ;
#15204 = DIRECTION ( 'NONE',  ( -0.000000000000000000, -1.000000000000000000, -0.000000000000000000 ) ) ;
#15205 = ORIENTED_EDGE ( 'NONE', *, *, #6318, .T. ) ;
#15206 = CARTESIAN_POINT ( 'NONE',  ( 40.34137639590981195, 41.05937500034139731, -29.30972558990011834 ) ) ;
#15207 = ORIENTED_EDGE ( 'NONE', *, *, #15040, .F. ) ;
#15208 = AXIS2_PLACEMENT_3D ( 'NONE', #8295, #1887, #8536 ) ;
#15209 =( LENGTH_UNIT ( ) NAMED_UNIT ( * ) SI_UNIT ( .MILLI., .METRE. ) );
#15210 = ORIENTED_EDGE ( 'NONE', *, *, #11870, .F. ) ;
#15211 = DIRECTION ( 'NONE',  ( 1.224646799147353207E-16, -1.000000000000000000, 0.000000000000000000 ) ) ;
#15212 = CARTESIAN_POINT ( 'NONE',  ( 30.81806926056964002, 26.55937500034139376, 42.41743335407647209 ) ) ;
#15213 = ORIENTED_EDGE ( 'NONE', *, *, #701, .F. ) ;
#15214 = CARTESIAN_POINT ( 'NONE',  ( 15.45084971874736723, 27.40000000000000213, -47.55282581475768211 ) ) ;
#15215 = DIRECTION ( 'NONE',  ( 0.9361168066628590134, -0.08189960831908912886, 0.3420201433256691570 ) ) ;
#15216 = CARTESIAN_POINT ( 'NONE',  ( 47.93512317712437465, 25.00000000000000000, -13.73719875613759989 ) ) ;
#15217 = CARTESIAN_POINT ( 'NONE',  ( 40.34137639590981905, 34.72187500034139873, 29.30972558990010768 ) ) ;
#15218 = CARTESIAN_POINT ( 'NONE',  ( 15.45084971874737789, 46.38125000068279746, 47.55282581475767500 ) ) ;
#15219 = CARTESIAN_POINT ( 'NONE',  ( 49.86468353124999453, 24.95937500034139234, -16.20201782572376104 ) ) ;
#15220 = CARTESIAN_POINT ( 'NONE',  ( 0.000000000000000000, 193.4213562373095385, -50.00000000000000000 ) ) ;
#15221 = CARTESIAN_POINT ( 'NONE',  ( 15.40903463028481113, 37.32187500034140015, -47.42413220539094709 ) ) ;
#15222 = PLANE ( 'NONE',  #16110 ) ;
#15223 = CARTESIAN_POINT ( 'NONE',  ( 15.45084971874736723, 33.39999999999999858, -47.55282581475768211 ) ) ;
#15224 = CARTESIAN_POINT ( 'NONE',  ( -49.86468353125000164, 35.85937500034140157, 0.000000000000000000 ) ) ;
#15225 = CARTESIAN_POINT ( 'NONE',  ( -3.210462471511496205E-15, 29.42187500034139092, -52.43083105670540789 ) ) ;
#15226 = EDGE_CURVE ( 'NONE', #9638, #14271, #7010, .T. ) ;
#15227 = CARTESIAN_POINT ( 'NONE',  ( -50.00000000000000000, 44.00000000000000711, 0.000000000000000000 ) ) ;
#15228 = ORIENTED_EDGE ( 'NONE', *, *, #13914, .T. ) ;
#15229 = APPLICATION_CONTEXT ( 'automotive_design' ) ;
#15230 = VERTEX_POINT ( 'NONE', #7098 ) ;
#15231 = UNCERTAINTY_MEASURE_WITH_UNIT (LENGTH_MEASURE( 1.000000000000000082E-05 ), #14936, 'distance_accuracy_value', 'NONE');
#15232 = CARTESIAN_POINT ( 'NONE',  ( -30.81806926056962226, 38.15937500034139163, 42.41743335407647209 ) ) ;
#15233 = ORIENTED_EDGE ( 'NONE', *, *, #10477, .F. ) ;
#15234 = ORIENTED_EDGE ( 'NONE', *, *, #14086, .T. ) ;
#15235 = EDGE_CURVE ( 'NONE', #13843, #384, #15724, .T. ) ;
#15236 = DIRECTION ( 'NONE',  ( -0.000000000000000000, -1.000000000000000000, -0.000000000000000000 ) ) ;
#15238 = EDGE_CURVE ( 'NONE', #3904, #9419, #6012, .T. ) ;
#15237 = CARTESIAN_POINT ( 'NONE',  ( -15.45084971874736368, 20.18125000068279817, 47.55282581475768211 ) ) ;
#15239 = VECTOR ( 'NONE', #11685, 1000.000000000000000 ) ;
#15240 = LINE ( 'NONE', #3865, #15770 ) ;
#15241 = CARTESIAN_POINT ( 'NONE',  ( 30.81806926056962936, 23.22187500034139163, -42.41743335407647209 ) ) ;
#15242 = DIRECTION ( 'NONE',  ( 0.000000000000000000, 1.000000000000000000, 0.000000000000000000 ) ) ;
#15243 = ADVANCED_FACE ( 'NONE', ( #8567 ), #2124, .T. ) ;
#15244 = CARTESIAN_POINT ( 'NONE',  ( -49.86468353124999453, 41.82187500034140015, -16.20201782572375393 ) ) ;
#15245 = CARTESIAN_POINT ( 'NONE',  ( -13.08647130699031713, 33.61029532559849287, 101.3333374614808662 ) ) ;
#15246 = CARTESIAN_POINT ( 'NONE',  ( 40.45084971874737079, 45.20000000000000284, -29.38926261462366440 ) ) ;
#15247 = CARTESIAN_POINT ( 'NONE',  ( 15.45084971874737789, 30.38125000068280102, 47.55282581475767500 ) ) ;
#15248 = CARTESIAN_POINT ( 'NONE',  ( -30.90169943749474513, 35.48125000068279888, -42.53254041760200721 ) ) ;
#15249 = ADVANCED_FACE ( 'NONE', ( #4283, #10604 ), #15816, .F. ) ;
#15250 = CARTESIAN_POINT ( 'NONE',  ( 30.81806926056962936, 33.22187500034139163, -42.41743335407647209 ) ) ;
#15251 = CARTESIAN_POINT ( 'NONE',  ( -1.790468199911976477, 98.25246584726777144, 9.080892972013895559 ) ) ;
#15252 = EDGE_LOOP ( 'NONE', ( #13352, #15441, #1273, #5784, #8331, #1185, #8931 ) ) ;
#15253 = ORIENTED_EDGE ( 'NONE', *, *, #10491, .T. ) ;
#15254 = CARTESIAN_POINT ( 'NONE',  ( -0.5000000000000000000, 39.99285568453590400, 101.0000000000000000 ) ) ;
#15255 = DIRECTION ( 'NONE',  ( 1.000000000000000000, 0.000000000000000000, 0.000000000000000000 ) ) ;
#15256 = STYLED_ITEM ( 'NONE', ( #1330 ), #8709 ) ;
#15257 = CARTESIAN_POINT ( 'NONE',  ( 0.000000000000000000, 53.82568851450475478, 0.000000000000000000 ) ) ;
#15258 = CARTESIAN_POINT ( 'NONE',  ( 0.000000000000000000, 20.00000000000000355, 0.000000000000000000 ) ) ;
#15259 = CARTESIAN_POINT ( 'NONE',  ( -49.86468353124999453, 29.75937500034139305, -16.20201782572375393 ) ) ;
#15260 = FACE_OUTER_BOUND ( 'NONE', #2378, .T. ) ;
#15261 = CARTESIAN_POINT ( 'NONE',  ( 40.34137639590981905, 48.72187500034139873, 29.30972558990010768 ) ) ;
#15262 = CARTESIAN_POINT ( 'NONE',  ( -49.99999999999999289, 40.09999999999999432, 16.24598481164533226 ) ) ;
#15263 = ADVANCED_FACE ( 'NONE', ( #1609 ), #6092, .T. ) ;
#15264 = CARTESIAN_POINT ( 'NONE',  ( -30.90169943749473447, 36.08125000068279320, 42.53254041760200721 ) ) ;
#15265 = DIRECTION ( 'NONE',  ( 0.000000000000000000, 0.000000000000000000, -1.000000000000000000 ) ) ;
#15266 = ORIENTED_EDGE ( 'NONE', *, *, #13021, .F. ) ;
#15267 = CARTESIAN_POINT ( 'NONE',  ( 40.34137639590981905, 48.72187500034139873, 29.30972558990010768 ) ) ;
#15268 = PRODUCT ( 'lid', 'lid', '', ( #464 ) ) ;
#15269 = ORIENTED_EDGE ( 'NONE', *, *, #8476, .F. ) ;
#15270 = CARTESIAN_POINT ( 'NONE',  ( -40.45084971874737789, 45.58125000068280031, -29.38926261462365730 ) ) ;
#15271 = ORIENTED_EDGE ( 'NONE', *, *, #8226, .F. ) ;
#15272 = VERTEX_POINT ( 'NONE', #11179 ) ;
#15273 = AXIS2_PLACEMENT_3D ( 'NONE', #12001, #3024, #2869 ) ;
#15274 = DIRECTION ( 'NONE',  ( 0.000000000000000000, 0.000000000000000000, -1.000000000000000000 ) ) ;
#15275 = CARTESIAN_POINT ( 'NONE',  ( 43.87482193696061472, 257.0000000000001137, -10.00000000000000000 ) ) ;
#15276 = DIRECTION ( 'NONE',  ( -0.000000000000000000, 0.7890408728378112135, -0.6143407043256575717 ) ) ;
#15277 = DIRECTION ( 'NONE',  ( -0.000000000000000000, 1.000000000000000000, -0.000000000000000000 ) ) ;
#15278 = AXIS2_PLACEMENT_3D ( 'NONE', #10136, #3817, #5333 ) ;
#15279 = CARTESIAN_POINT ( 'NONE',  ( -17.34476375915448187, 20.17423772944842142, 101.0000000000000000 ) ) ;
#15280 = DIRECTION ( 'NONE',  ( 0.000000000000000000, -0.000000000000000000, 1.000000000000000000 ) ) ;
#15281 = AXIS2_PLACEMENT_3D ( 'NONE', #702, #4545, #7124 ) ;
#15282 = VECTOR ( 'NONE', #2958, 1000.000000000000000 ) ;
#15283 = FACE_OUTER_BOUND ( 'NONE', #2439, .T. ) ;
#15284 = CARTESIAN_POINT ( 'NONE',  ( 50.00000000000000000, 24.78125000068279959, -6.123233995736766085E-15 ) ) ;
#15285 = AXIS2_PLACEMENT_3D ( 'NONE', #3126, #3602, #7265 ) ;
#15286 = ADVANCED_FACE ( 'NONE', ( #847 ), #7183, .F. ) ;
#15287 = PRODUCT_DEFINITION_FORMATION_WITH_SPECIFIED_SOURCE ( 'ANY', '', #15268, .NOT_KNOWN. ) ;
#15288 = DIRECTION ( 'NONE',  ( 0.000000000000000000, 0.000000000000000000, 1.000000000000000000 ) ) ;
#15289 = CARTESIAN_POINT ( 'NONE',  ( -40.45084971874737789, 41.58125000068280031, -29.38926261462365730 ) ) ;
#15290 =( BOUNDED_CURVE ( )  B_SPLINE_CURVE ( 2, ( #12424, #9767, #7272, #14643, #12328, #8578, #6112, #3526, #11100, #9847, #7434, #5779, #3271 ),
 .UNSPECIFIED., .F., .T. ) 
 B_SPLINE_CURVE_WITH_KNOTS ( ( 3, 2, 2, 2, 2, 2, 3 ),
 ( 0.7500000000000000000, 0.7533333333333332993, 0.7600000000000000089, 0.7666666666666667185, 0.7733333333333333171, 0.7800000000000000266, 0.7833333333333333259 ),
 .UNSPECIFIED. ) 
 CURVE ( )  GEOMETRIC_REPRESENTATION_ITEM ( )  RATIONAL_B_SPLINE_CURVE ( ( 0.9755282581475768211, 0.9755282581475768211, 1.000000000000000000, 0.9510565162951535312, 1.000000000000000000, 0.9510565162951535312, 1.000000000000000000, 0.9510565162951535312, 1.000000000000000000, 0.9510565162951535312, 1.000000000000000000, 0.9755282581475768211, 0.9755282581475768211 ) ) 
 REPRESENTATION_ITEM ( '' )  );
#15291 = CARTESIAN_POINT ( 'NONE',  ( 30.90169943749475223, 20.69999999999999574, 42.53254041760199300 ) ) ;
#15292 = CARTESIAN_POINT ( 'NONE',  ( 50.00000000000000000, 46.78125000068279604, -6.123233995736766085E-15 ) ) ;
#15293 = SURFACE_STYLE_FILL_AREA ( #11554 ) ;
#15294 = ORIENTED_EDGE ( 'NONE', *, *, #4180, .T. ) ;
#15295 = CARTESIAN_POINT ( 'NONE',  ( 40.34137639590981195, 45.05937500034139731, -29.30972558990011834 ) ) ;
#15296 = ORIENTED_EDGE ( 'NONE', *, *, #11096, .F. ) ;
#15297 = AXIS2_PLACEMENT_3D ( 'NONE', #15083, #11437, #2693 ) ;
#15298 = AXIS2_PLACEMENT_3D ( 'NONE', #10567, #6748, #10807 ) ;
#15299 = VECTOR ( 'NONE', #8006, 1000.000000000000000 ) ;
#15300 = CYLINDRICAL_SURFACE ( 'NONE', #11288, 17.50000000000000000 ) ;
#15301 = CARTESIAN_POINT ( 'NONE',  ( 43.87482193696061472, 257.0000000000001137, 10.00000000000000178 ) ) ;
#15302 = CARTESIAN_POINT ( 'NONE',  ( -30.81806926056963292, 31.55937500034139731, -42.41743335407647209 ) ) ;
#15303 = ORIENTED_EDGE ( 'NONE', *, *, #5021, .T. ) ;
#15304 = DIRECTION ( 'NONE',  ( 0.5877852522924688072, 0.8090169943749505599, 0.000000000000000000 ) ) ;
#15305 = FACE_OUTER_BOUND ( 'NONE', #8309, .T. ) ;
#15306 = CARTESIAN_POINT ( 'NONE',  ( 0.000000000000000000, 217.0000000000000284, 45.00000000000000000 ) ) ;
#15307 = CARTESIAN_POINT ( 'NONE',  ( 30.81806926056964002, 34.62187500034139731, 42.41743335407646498 ) ) ;
#15308 = DIRECTION ( 'NONE',  ( -0.000000000000000000, -1.000000000000000000, -0.000000000000000000 ) ) ;
#15309 = EDGE_CURVE ( 'NONE', #11113, #8227, #675, .T. ) ;
#15310 = CARTESIAN_POINT ( 'NONE',  ( -30.81806926056962226, 26.15937500034139163, 42.41743335407647209 ) ) ;
#15311 = VECTOR ( 'NONE', #198, 1000.000000000000114 ) ;
#15312 = CARTESIAN_POINT ( 'NONE',  ( 7.919222016226809657, 43.44874571845315359, -50.00000000000000000 ) ) ;
#15313 = CARTESIAN_POINT ( 'NONE',  ( 15.40903463028481113, 31.32187500034139305, -47.42413220539094709 ) ) ;
#15314 = CIRCLE ( 'NONE', #9754, 9.080892972013911546 ) ;
#15315 = DIRECTION ( 'NONE',  ( 0.000000000000000000, 0.000000000000000000, -1.000000000000000000 ) ) ;
#15316 = CARTESIAN_POINT ( 'NONE',  ( -30.90169943749473802, 32.30000000000000426, 42.53254041760200721 ) ) ;
#15317 = CARTESIAN_POINT ( 'NONE',  ( -49.86468353124999453, 37.95937500034140299, 16.20201782572377525 ) ) ;
#15318 = CARTESIAN_POINT ( 'NONE',  ( 15.40903463028481113, 33.32187500034139305, -47.42413220539094709 ) ) ;
#15319 = CARTESIAN_POINT ( 'NONE',  ( -49.99999999999999289, 41.90000000000001279, -16.24598481164531449 ) ) ;
#15320 = VERTEX_POINT ( 'NONE', #4607 ) ;
#15321 = CARTESIAN_POINT ( 'NONE',  ( 15.40903463028481113, 33.25937500034140015, -47.42413220539094709 ) ) ;
#15322 = AXIS2_PLACEMENT_3D ( 'NONE', #2932, #5603, #2851 ) ;
#15323 = EDGE_CURVE ( 'NONE', #5006, #10042, #11248, .T. ) ;
#15324 = ORIENTED_EDGE ( 'NONE', *, *, #10540, .F. ) ;
#15325 = ORIENTED_EDGE ( 'NONE', *, *, #12924, .F. ) ;
#15326 = CARTESIAN_POINT ( 'NONE',  ( 23.90010208165381300, 283.0244618719127629, -9.450051040827696980 ) ) ;
#15327 = CARTESIAN_POINT ( 'NONE',  ( 40.34137639590981195, 49.05937500034139731, -29.30972558990011834 ) ) ;
#15328 = DIRECTION ( 'NONE',  ( 0.000000000000000000, 0.000000000000000000, 1.000000000000000000 ) ) ;
#15329 = CARTESIAN_POINT ( 'NONE',  ( 49.86468353125001585, 22.82187500034138949, 16.20201782572375038 ) ) ;
#15330 = PLANE ( 'NONE',  #15297 ) ;
#15331 = CARTESIAN_POINT ( 'NONE',  ( -15.40903463028481646, 41.52187500034139589, -47.42413220539093999 ) ) ;
#15332 = CARTESIAN_POINT ( 'NONE',  ( 30.81806926056964002, 42.55937500034139020, 42.41743335407646498 ) ) ;
#15333 = DIRECTION ( 'NONE',  ( 0.000000000000000000, 1.000000000000000000, 0.000000000000000000 ) ) ;
#15334 = CARTESIAN_POINT ( 'NONE',  ( 30.90169943749475578, 46.69999999999999574, 42.53254041760200010 ) ) ;
#15335 = CARTESIAN_POINT ( 'NONE',  ( 15.45084971874737789, 28.38125000068279746, 47.55282581475767500 ) ) ;
#15336 = EDGE_CURVE ( 'NONE', #4175, #13132, #12867, .T. ) ;
#15337 = APPLICATION_CONTEXT ( 'automotive_design' ) ;
#15338 = CARTESIAN_POINT ( 'NONE',  ( -3.111920190527341144E-15, 35.28125000068280315, -50.00000000000000000 ) ) ;
#15339 = CARTESIAN_POINT ( 'NONE',  ( 40.34137639590981905, 36.72187500034139163, 29.30972558990010768 ) ) ;
#15340 = CARTESIAN_POINT ( 'NONE',  ( 5.000000000000000000, 99.58041009241399877, 7.580410092413963241 ) ) ;
#15341 = EDGE_LOOP ( 'NONE', ( #13063, #10914, #10183, #4412 ) ) ;
#15342 = CARTESIAN_POINT ( 'NONE',  ( 15.45084971874736723, 37.18125000068280173, -47.55282581475768211 ) ) ;
#15343 = ORIENTED_EDGE ( 'NONE', *, *, #4345, .T. ) ;
#15344 = CARTESIAN_POINT ( 'NONE',  ( -12.41734070063146156, 34.35344015107588689, 101.3333374614808662 ) ) ;
#15345 = CARTESIAN_POINT ( 'NONE',  ( 30.90169943749473802, 45.29999999999999005, -42.53254041760200721 ) ) ;
#15346 = EDGE_CURVE ( 'NONE', #14468, #11210, #3267, .T. ) ;
#15347 = FACE_OUTER_BOUND ( 'NONE', #12606, .T. ) ;
#15348 = CARTESIAN_POINT ( 'NONE',  ( -30.81806926056963292, 49.62187500034139020, -42.41743335407646498 ) ) ;
#15349 = CARTESIAN_POINT ( 'NONE',  ( -40.34137639590981905, 33.65937500034139873, -29.30972558990011478 ) ) ;
#15350 = LINE ( 'NONE', #5151, #10614 ) ;
#15351 = CARTESIAN_POINT ( 'NONE',  ( -15.40903463028481646, 47.52187500034139589, -47.42413220539093999 ) ) ;
#15352 = SHAPE_DEFINITION_REPRESENTATION ( #9190, #329 ) ;
#15353 = LINE ( 'NONE', #9122, #5180 ) ;
#15354 = CIRCLE ( 'NONE', #2879, 45.00000000000000711 ) ;
#15355 = DIRECTION ( 'NONE',  ( 0.000000000000000000, 1.000000000000000000, 0.000000000000000000 ) ) ;
#15356 = CARTESIAN_POINT ( 'NONE',  ( 7.919222016226809657, 29.22999571913594963, -50.00000000000000000 ) ) ;
#15357 = VERTEX_POINT ( 'NONE', #2257 ) ;
#15358 = EDGE_CURVE ( 'NONE', #5867, #4422, #2669, .T. ) ;
#15359 = CARTESIAN_POINT ( 'NONE',  ( 49.86468353124999453, 47.02187500034139589, -16.20201782572376459 ) ) ;
#15360 = ORIENTED_EDGE ( 'NONE', *, *, #2912, .T. ) ;
#15361 = PLANE ( 'NONE',  #6284 ) ;
#15362 = ORIENTED_EDGE ( 'NONE', *, *, #13064, .T. ) ;
#15363 = ORIENTED_EDGE ( 'NONE', *, *, #8269, .T. ) ;
#15364 = CARTESIAN_POINT ( 'NONE',  ( -3.111920190527341144E-15, 35.28125000068280315, -50.00000000000000000 ) ) ;
#15365 = CARTESIAN_POINT ( 'NONE',  ( 7.919222016226875382, 39.22999571913595673, -49.99999999999997158 ) ) ;
#15366 = DIRECTION ( 'NONE',  ( -0.9135454576426059736, 0.4067366430757887730, 0.000000000000000000 ) ) ;
#15367 = DIRECTION ( 'NONE',  ( 0.000000000000000000, 0.000000000000000000, -1.000000000000000000 ) ) ;
#15368 = CARTESIAN_POINT ( 'NONE',  ( -15.40903463028480580, 48.25937500034140015, 47.42413220539094709 ) ) ;
#15369 = CARTESIAN_POINT ( 'NONE',  ( 0.000000000000000000, 252.0000000000000000, 0.000000000000000000 ) ) ;
#15370 = DIRECTION ( 'NONE',  ( 0.000000000000000000, 0.000000000000000000, -1.000000000000000000 ) ) ;
#15371 = SHAPE_REPRESENTATION_RELATIONSHIP ( 'NONE' , 'NONE' ,  #13393, #12174 ) ;
#15372 = DIRECTION ( 'NONE',  ( 5.069245582283711292E-17, 1.000000000000000000, -8.780190904559502465E-17 ) ) ;
#15373 = CARTESIAN_POINT ( 'NONE',  ( 9.657523855033129090E-15, 38.28125000068279604, 52.57311121191334990 ) ) ;
#15374 = CARTESIAN_POINT ( 'NONE',  ( 3.505380114644273348, 97.73782665365219202, 8.566253778398346341 ) ) ;
#15375 = CARTESIAN_POINT ( 'NONE',  ( -50.00000000000000000, 22.00000000000000355, 0.000000000000000000 ) ) ;
#15376 = CARTESIAN_POINT ( 'NONE',  ( 0.000000000000000000, 0.000000000000000000, 5.000000000000000000 ) ) ;
#15377 = EDGE_CURVE ( 'NONE', #4340, #8347, #6024, .T. ) ;
#15378 = ORIENTED_EDGE ( 'NONE', *, *, #5864, .F. ) ;
#15379 = EDGE_CURVE ( 'NONE', #3842, #1639, #9762, .T. ) ;
#15380 = CARTESIAN_POINT ( 'NONE',  ( -30.81806926056963292, 35.55937500034139020, -42.41743335407647209 ) ) ;
#15381 =( GEOMETRIC_REPRESENTATION_CONTEXT ( 3 ) GLOBAL_UNCERTAINTY_ASSIGNED_CONTEXT ( ( #4441 ) ) GLOBAL_UNIT_ASSIGNED_CONTEXT ( ( #7325, #987, #14954 ) ) REPRESENTATION_CONTEXT ( 'NONE', 'WORKASPACE' ) );
#15382 = ORIENTED_EDGE ( 'NONE', *, *, #5722, .F. ) ;
#15383 = CARTESIAN_POINT ( 'NONE',  ( 50.00000000000000711, 42.68125000068280173, 16.24598481164530739 ) ) ;
#15384 = CARTESIAN_POINT ( 'NONE',  ( 0.000000000000000000, 274.0000000000000000, 87.81953344283027718 ) ) ;
#15385 = CARTESIAN_POINT ( 'NONE',  ( 15.40903463028482356, 30.45937500034139589, 47.42413220539093999 ) ) ;
#15386 = ORIENTED_EDGE ( 'NONE', *, *, #14987, .F. ) ;
#15387 = CARTESIAN_POINT ( 'NONE',  ( 0.000000000000000000, 20.00000000000000355, 0.000000000000000000 ) ) ;
#15388 = CARTESIAN_POINT ( 'NONE',  ( -16.94841605670512052, 27.00700085982962051, 93.71793596878799804 ) ) ;
#15389 = CARTESIAN_POINT ( 'NONE',  ( 47.69912754770714258, 25.00000000000000711, -14.53642574140263299 ) ) ;
#15390 = CARTESIAN_POINT ( 'NONE',  ( 30.81806926056962936, 31.22187500034139518, -42.41743335407646498 ) ) ;
#15391 =( BOUNDED_CURVE ( )  B_SPLINE_CURVE ( 2, ( #1643, #9225, #9305, #9134, #2901, #13117, #15524, #1566, #308, #6740, #14279, #15443, #5407 ),
 .UNSPECIFIED., .F., .F. ) 
 B_SPLINE_CURVE_WITH_KNOTS ( ( 3, 2, 2, 2, 2, 2, 3 ),
 ( 0.1833333333333333481, 0.1866666666666666752, 0.1933333333333333293, 0.2000000000000000111, 0.2066666666666666652, 0.2133333333333333470, 0.2166666666666666741 ),
 .UNSPECIFIED. ) 
 CURVE ( )  GEOMETRIC_REPRESENTATION_ITEM ( )  RATIONAL_B_SPLINE_CURVE ( ( 0.9755282581475767101, 0.9755282581475768211, 1.000000000000000000, 0.9510565162951535312, 1.000000000000000000, 0.9510565162951535312, 1.000000000000000000, 0.9510565162951535312, 1.000000000000000000, 0.9510565162951535312, 1.000000000000000000, 0.9755282581475768211, 0.9755282581475768211 ) ) 
 REPRESENTATION_ITEM ( '' )  );
#15392 = CARTESIAN_POINT ( 'NONE',  ( -1.240322475938754499E-13, 38.28125000068280315, 50.00000000000000000 ) ) ;
#15393 = CIRCLE ( 'NONE', #13004, 16.50000000000000711 ) ;
#15394 = CARTESIAN_POINT ( 'NONE',  ( -30.81806926056962226, 22.15937500034139163, 42.41743335407647209 ) ) ;
#15395 = DIRECTION ( 'NONE',  ( 0.000000000000000000, 0.000000000000000000, -1.000000000000000000 ) ) ;
#15396 = EDGE_CURVE ( 'NONE', #2225, #1658, #3440, .T. ) ;
#15397 = CARTESIAN_POINT ( 'NONE',  ( -49.86468353125000164, 31.92187500034139447, 0.000000000000000000 ) ) ;
#15398 = LINE ( 'NONE', #182, #13978 ) ;
#15399 = CARTESIAN_POINT ( 'NONE',  ( -40.45084971874737079, 28.20000000000000284, 29.38926261462367151 ) ) ;
#15400 = EDGE_CURVE ( 'NONE', #14510, #562, #926, .T. ) ;
#15401 = CARTESIAN_POINT ( 'NONE',  ( 40.34137639590981195, 33.05937500034139731, -29.30972558990011834 ) ) ;
#15402 = CARTESIAN_POINT ( 'NONE',  ( -30.81806926056963292, 31.62187500034139731, -42.41743335407647209 ) ) ;
#15403 = ORIENTED_EDGE ( 'NONE', *, *, #4586, .F. ) ;
#15404 = EDGE_CURVE ( 'NONE', #15953, #1138, #266, .T. ) ;
#15405 = UNCERTAINTY_MEASURE_WITH_UNIT (LENGTH_MEASURE( 1.000000000000000082E-05 ), #2571, 'distance_accuracy_value', 'NONE');
#15406 = CARTESIAN_POINT ( 'NONE',  ( -49.86468353124999453, 35.95937500034139589, 16.20201782572377169 ) ) ;
#15407 = ORIENTED_EDGE ( 'NONE', *, *, #2445, .F. ) ;
#15408 = VERTEX_POINT ( 'NONE', #12740 ) ;
#15409 = CARTESIAN_POINT ( 'NONE',  ( 20.51073895446738504, 285.3889217077638705, -7.755369477227150199 ) ) ;
#15410 = CARTESIAN_POINT ( 'NONE',  ( 30.81806926056962936, 47.15937500034138452, -42.41743335407647209 ) ) ;
#15411 = DIRECTION ( 'NONE',  ( 0.000000000000000000, 0.000000000000000000, 1.000000000000000000 ) ) ;
#15412 = CARTESIAN_POINT ( 'NONE',  ( -30.81806926056963292, 25.62187500034139731, -42.41743335407647209 ) ) ;
#15413 = CARTESIAN_POINT ( 'NONE',  ( 40.34137639590981905, 34.72187500034139873, 29.30972558990010768 ) ) ;
#15414 = CARTESIAN_POINT ( 'NONE',  ( -49.86468353124999453, 39.95937500034139589, 16.20201782572377169 ) ) ;
#15415 = CARTESIAN_POINT ( 'NONE',  ( 5.510910596163089556E-15, 217.0000000000000284, -45.00000000000000000 ) ) ;
#15416 = CARTESIAN_POINT ( 'NONE',  ( -49.99999999999999289, 45.89999999999999858, -16.24598481164531449 ) ) ;
#15417 = CARTESIAN_POINT ( 'NONE',  ( -49.99999999999999289, 23.68125000068279462, -16.24598481164531449 ) ) ;
#15418 = CARTESIAN_POINT ( 'NONE',  ( 12.00283417906081773, 35.24790003054248899, 93.01444432686068353 ) ) ;
#15419 = CARTESIAN_POINT ( 'NONE',  ( -49.86468353124999453, 26.02187500034139944, 16.20201782572377525 ) ) ;
#15420 = LINE ( 'NONE', #6636, #11013 ) ;
#15421 = VERTEX_POINT ( 'NONE', #5190 ) ;
#15422 = CARTESIAN_POINT ( 'NONE',  ( -40.45084971874737789, 37.58125000068280031, -29.38926261462365730 ) ) ;
#15423 = VERTEX_POINT ( 'NONE', #15306 ) ;
#15424 = DIRECTION ( 'NONE',  ( -2.312964634635742464E-16, 0.000000000000000000, 1.000000000000000000 ) ) ;
#15425 = FACE_BOUND ( 'NONE', #12752, .T. ) ;
#15426 = CARTESIAN_POINT ( 'NONE',  ( -50.00000000000000000, 24.00000000000000000, 0.000000000000000000 ) ) ;
#15427 = CARTESIAN_POINT ( 'NONE',  ( 49.86468353125001585, 48.82187500034139305, 16.20201782572375038 ) ) ;
#15428 = CARTESIAN_POINT ( 'NONE',  ( 49.86468353125001585, 26.75937500034139660, 16.20201782572375038 ) ) ;
#15429 = CARTESIAN_POINT ( 'NONE',  ( 0.5000000000000000000, 39.99285568453590400, 101.0000000000000000 ) ) ;
#15430 = LINE ( 'NONE', #14097, #11150 ) ;
#15431 = CARTESIAN_POINT ( 'NONE',  ( 15.40903463028482356, 44.52187500034139589, 47.42413220539093999 ) ) ;
#15432 = APPLICATION_PROTOCOL_DEFINITION ( 'draft international standard', 'automotive_design', 1998, #2077 ) ;
#15433 = CYLINDRICAL_SURFACE ( 'NONE', #9683, 45.00000000000000711 ) ;
#15434 = FACE_OUTER_BOUND ( 'NONE', #10264, .T. ) ;
#15435 = CARTESIAN_POINT ( 'NONE',  ( -17.44929222242214095, 21.16875962481669760, 101.0000000000000000 ) ) ;
#15436 = ORIENTED_EDGE ( 'NONE', *, *, #11589, .F. ) ;
#15437 = EDGE_CURVE ( 'NONE', #11113, #12621, #14403, .T. ) ;
#15438 = CARTESIAN_POINT ( 'NONE',  ( 49.86468353125000164, 48.92187500034139447, -6.106662507704105588E-15 ) ) ;
#15439 = ORIENTED_EDGE ( 'NONE', *, *, #1549, .F. ) ;
#15440 = LINE ( 'NONE', #2721, #11848 ) ;
#15441 = ORIENTED_EDGE ( 'NONE', *, *, #6942, .T. ) ;
#15442 = EDGE_LOOP ( 'NONE', ( #7446, #414, #11854, #3857 ) ) ;
#15443 = CARTESIAN_POINT ( 'NONE',  ( -7.919222016226816763, 43.33250428222963535, -49.99999999999999289 ) ) ;
#15444 = DIRECTION ( 'NONE',  ( -0.000000000000000000, -1.000000000000000000, -0.000000000000000000 ) ) ;
#15445 = EDGE_CURVE ( 'NONE', #5291, #495, #4614, .T. ) ;
#15446 = EDGE_CURVE ( 'NONE', #5162, #6674, #14137, .T. ) ;
#15447 = CARTESIAN_POINT ( 'NONE',  ( -49.99999999999999289, 27.89999999999999858, -16.24598481164531449 ) ) ;
#15448 = CARTESIAN_POINT ( 'NONE',  ( 49.86468353125000164, 48.85937500034139447, -6.106662507704105588E-15 ) ) ;
#15449 = CARTESIAN_POINT ( 'NONE',  ( -15.45084971874737256, 25.38125000068279746, -47.55282581475767500 ) ) ;
#15450 = DIRECTION ( 'NONE',  ( 0.000000000000000000, 0.000000000000000000, 1.000000000000000000 ) ) ;
#15451 = CARTESIAN_POINT ( 'NONE',  ( -3.210462471511496205E-15, 23.42187500034139802, -52.43083105670540789 ) ) ;
#15452 = EDGE_CURVE ( 'NONE', #2396, #5969, #2752, .T. ) ;
#15453 = PLANE ( 'NONE',  #8337 ) ;
#15454 = CARTESIAN_POINT ( 'NONE',  ( -50.00000000000000000, 41.78125000068280315, 0.000000000000000000 ) ) ;
#15455 = CARTESIAN_POINT ( 'NONE',  ( -15.45084971874737256, 37.38125000068279746, -47.55282581475767500 ) ) ;
#15456 =( BOUNDED_CURVE ( )  B_SPLINE_CURVE ( 2, ( #765, #13400, #5856, #12421, #1012, #2095, #12073, #2258, #6109, #16234, #4868, #3186, #13324 ),
 .UNSPECIFIED., .F., .F. ) 
 B_SPLINE_CURVE_WITH_KNOTS ( ( 3, 2, 2, 2, 2, 2, 3 ),
 ( 0.1499999999999999944, 0.1533333333333333215, 0.1600000000000000033, 0.1666666666666666574, 0.1733333333333333393, 0.1799999999999999933, 0.1833333333333333481 ),
 .UNSPECIFIED. ) 
 CURVE ( )  GEOMETRIC_REPRESENTATION_ITEM ( )  RATIONAL_B_SPLINE_CURVE ( ( 0.9755282581475768211, 0.9755282581475768211, 1.000000000000000000, 0.9510565162951535312, 1.000000000000000000, 0.9510565162951535312, 1.000000000000000000, 0.9510565162951535312, 1.000000000000000000, 0.9510565162951535312, 1.000000000000000000, 0.9755282581475765991, 0.9755282581475767101 ) ) 
 REPRESENTATION_ITEM ( '' )  );
#15457 = CARTESIAN_POINT ( 'NONE',  ( -3.219174618344376363E-15, 23.50000000000000000, -52.57311121191334990 ) ) ;
#15458 = ORIENTED_EDGE ( 'NONE', *, *, #4378, .T. ) ;
#15459 = EDGE_CURVE ( 'NONE', #4499, #895, #11900, .T. ) ;
#15460 = CARTESIAN_POINT ( 'NONE',  ( -40.34137639590981195, 38.05937500034139731, 29.30972558990012189 ) ) ;
#15461 = ORIENTED_EDGE ( 'NONE', *, *, #6958, .T. ) ;
#15462 = CARTESIAN_POINT ( 'NONE',  ( 0.000000000000000000, 52.00000000000000711, 0.000000000000000000 ) ) ;
#15463 = CARTESIAN_POINT ( 'NONE',  ( 9.735664389687646693E-15, 272.0000000000000000, 79.49773270518484480 ) ) ;
#15464 = CARTESIAN_POINT ( 'NONE',  ( -30.81806926056962226, 28.15937500034139518, 42.41743335407647919 ) ) ;
#15466 = VERTEX_POINT ( 'NONE', #4343 ) ;
#15465 = VECTOR ( 'NONE', #2915, 1000.000000000000000 ) ;
#15467 = DIRECTION ( 'NONE',  ( 1.000000000000000000, 0.000000000000000000, 0.000000000000000000 ) ) ;
#15468 = DIRECTION ( 'NONE',  ( -6.938893903907231459E-18, 1.000000000000000000, 5.551115123125782702E-17 ) ) ;
#15469 = DIRECTION ( 'NONE',  ( -0.4067366430757887175, -0.9135454576426059736, 0.000000000000000000 ) ) ;
#15470 = CARTESIAN_POINT ( 'NONE',  ( 30.81806926056962936, 33.22187500034139163, -42.41743335407646498 ) ) ;
#15471 = CARTESIAN_POINT ( 'NONE',  ( -25.00000000000000355, 312.0000000000000568, -2.499999999999998668 ) ) ;
#15472 = CARTESIAN_POINT ( 'NONE',  ( 5.716386541834933332, 5.919903133645938453, 98.79670695971100258 ) ) ;
#15473 = CARTESIAN_POINT ( 'NONE',  ( -46.85365039762112360, 20.00000000000000355, 17.06523097087215390 ) ) ;
#15474 = CARTESIAN_POINT ( 'NONE',  ( 40.34137639590981195, 27.12187500034139731, -29.30972558990011834 ) ) ;
#15475 = DIRECTION ( 'NONE',  ( 0.000000000000000000, 1.000000000000000000, 0.000000000000000000 ) ) ;
#15476 = CARTESIAN_POINT ( 'NONE',  ( 50.00000000000000711, 28.89999999999999858, 16.24598481164530739 ) ) ;
#15477 = CARTESIAN_POINT ( 'NONE',  ( -49.86468353124999453, 33.75937500034140015, -16.20201782572375393 ) ) ;
#15478 = CARTESIAN_POINT ( 'NONE',  ( -40.34137639590981195, 28.12187500034139731, 29.30972558990012189 ) ) ;
#15479 = VECTOR ( 'NONE', #9835, 1000.000000000000000 ) ;
#15480 = CARTESIAN_POINT ( 'NONE',  ( 30.90169943749473802, 39.30000000000000426, -42.53254041760200721 ) ) ;
#15481 = VERTEX_POINT ( 'NONE', #14381 ) ;
#15482 = CARTESIAN_POINT ( 'NONE',  ( -30.81806926056963292, 27.55937500034139376, -42.41743335407646498 ) ) ;
#15483 = VERTEX_POINT ( 'NONE', #10584 ) ;
#15484 = CARTESIAN_POINT ( 'NONE',  ( 26.77784341583361183, 282.2553694771637538, -10.88892170791706171 ) ) ;
#15486 =( BOUNDED_CURVE ( )  B_SPLINE_CURVE ( 2, ( #6836, #9480, #6672, #15626, #4251, #9317, #14204, #4075, #8147, #5585, #639, #11721, #14528 ),
 .UNSPECIFIED., .F., .F. ) 
 B_SPLINE_CURVE_WITH_KNOTS ( ( 3, 2, 2, 2, 2, 2, 3 ),
 ( 0.9500000000000000666, 0.9533333333333333659, 0.9599999999999999645, 0.9666666666666666741, 0.9733333333333333837, 0.9799999999999999822, 0.9833333333333333925 ),
 .UNSPECIFIED. ) 
 CURVE ( )  GEOMETRIC_REPRESENTATION_ITEM ( )  RATIONAL_B_SPLINE_CURVE ( ( 0.9755282581475768211, 0.9755282581475771542, 1.000000000000000000, 0.9510565162951535312, 1.000000000000000000, 0.9510565162951535312, 1.000000000000000000, 0.9510565162951535312, 1.000000000000000000, 0.9510565162951535312, 1.000000000000000000, 0.9755282581475763770, 0.9755282581475768211 ) ) 
 REPRESENTATION_ITEM ( '' )  );
#15485 = CARTESIAN_POINT ( 'NONE',  ( 15.45084971874736723, 21.18125000068279817, -47.55282581475768211 ) ) ;
#15487 = DIRECTION ( 'NONE',  ( 0.000000000000000000, 0.000000000000000000, 1.000000000000000000 ) ) ;
#15488 = CARTESIAN_POINT ( 'NONE',  ( 29.67274705320743422, 282.0000000000000000, 11.84549410641326617 ) ) ;
#15489 = VECTOR ( 'NONE', #65, 999.9999999999998863 ) ;
#15490 = CARTESIAN_POINT ( 'NONE',  ( 40.34137639590981905, 36.72187500034139163, 29.30972558990010768 ) ) ;
#15491 = CARTESIAN_POINT ( 'NONE',  ( -3.210462471511496205E-15, 43.35937500034139447, -52.43083105670540789 ) ) ;
#15492 = CARTESIAN_POINT ( 'NONE',  ( 5.179451399591075145, 14.52044592729181538, 102.0000000000000142 ) ) ;
#15493 = CARTESIAN_POINT ( 'NONE',  ( -15.45084971874737256, 41.60000000000000142, -47.55282581475767500 ) ) ;
#15494 = ADVANCED_FACE ( 'NONE', ( #499 ), #5359, .F. ) ;
#15495 = CARTESIAN_POINT ( 'NONE',  ( -40.34137639590981905, 49.65937500034139873, -29.30972558990011478 ) ) ;
#15496 = CARTESIAN_POINT ( 'NONE',  ( -30.81806926056962226, 48.22187500034139163, 42.41743335407647919 ) ) ;
#15497 = CARTESIAN_POINT ( 'NONE',  ( -30.81806926056963292, 29.62187500034139376, -42.41743335407647209 ) ) ;
#15498 = AXIS2_PLACEMENT_3D ( 'NONE', #3994, #1495, #238 ) ;
#15499 = DIRECTION ( 'NONE',  ( 5.069245582283711292E-17, 1.000000000000000000, -8.780190904559503697E-17 ) ) ;
#15500 = ORIENTED_EDGE ( 'NONE', *, *, #711, .T. ) ;
#15501 = CARTESIAN_POINT ( 'NONE',  ( 15.45084971874737789, 40.38125000068280457, 47.55282581475767500 ) ) ;
#15502 = ORIENTED_EDGE ( 'NONE', *, *, #590, .T. ) ;
#15503 = CARTESIAN_POINT ( 'NONE',  ( 7.500000000000000000, 40.00000000000000711, 39.29058411375427795 ) ) ;
#15504 = CARTESIAN_POINT ( 'NONE',  ( 9.366734789577542680E-15, 82.00000000000001421, -2.024759949320127682E-14 ) ) ;
#15505 = CARTESIAN_POINT ( 'NONE',  ( 15.45084971874736723, 31.18125000068279817, -47.55282581475768211 ) ) ;
#15506 = CARTESIAN_POINT ( 'NONE',  ( -40.34137639590981905, 45.72187500034139873, -29.30972558990011478 ) ) ;
#15507 = CARTESIAN_POINT ( 'NONE',  ( 30.81806926056962936, 25.15937500034139518, -42.41743335407647209 ) ) ;
#15508 = CARTESIAN_POINT ( 'NONE',  ( 0.000000000000000000, 20.00000000000000355, 0.000000000000000000 ) ) ;
#15509 = AXIS2_PLACEMENT_3D ( 'NONE', #16040, #2151, #4925 ) ;
#15510 = CARTESIAN_POINT ( 'NONE',  ( 49.86468353125001585, 42.82187500034139305, 16.20201782572375038 ) ) ;
#15511 = DIRECTION ( 'NONE',  ( 0.000000000000000000, 0.000000000000000000, 1.000000000000000000 ) ) ;
#15512 = CARTESIAN_POINT ( 'NONE',  ( 48.35726954556789536, 24.99999999999999645, -12.16803787670825265 ) ) ;
#15513 = CARTESIAN_POINT ( 'NONE',  ( 49.86468353124999453, 47.02187500034139589, -16.20201782572376459 ) ) ;
#15514 = LINE ( 'NONE', #7960, #331 ) ;
#15515 = ORIENTED_EDGE ( 'NONE', *, *, #15452, .T. ) ;
#15516 = CARTESIAN_POINT ( 'NONE',  ( 49.86468353125001585, 48.82187500034139305, 16.20201782572375038 ) ) ;
#15517 = VERTEX_POINT ( 'NONE', #1753 ) ;
#15518 = DIRECTION ( 'NONE',  ( 0.7431448254773862505, 0.6691306063588672304, 0.000000000000000000 ) ) ;
#15519 = ORIENTED_EDGE ( 'NONE', *, *, #8241, .F. ) ;
#15520 = ORIENTED_EDGE ( 'NONE', *, *, #3000, .T. ) ;
#15522 = EDGE_CURVE ( 'NONE', #7238, #12589, #2577, .T. ) ;
#15521 = CONICAL_SURFACE ( 'NONE', #14445, 62.01141590572476758, 0.08726646259971666819 ) ;
#15523 = ADVANCED_FACE ( 'NONE', ( #1829 ), #9251, .F. ) ;
#15524 = CARTESIAN_POINT ( 'NONE',  ( -50.00000000000000000, 43.78125000068280315, 0.000000000000000000 ) ) ;
#15525 = PLANE ( 'NONE',  #12082 ) ;
#15526 = CARTESIAN_POINT ( 'NONE',  ( 49.99999999999999289, 29.10000000000000142, -16.24598481164532160 ) ) ;
#15527 = CARTESIAN_POINT ( 'NONE',  ( 40.45084971874737789, 26.80000000000000071, 29.38926261462365375 ) ) ;
#15528 = CARTESIAN_POINT ( 'NONE',  ( 15.40903463028481113, 47.25937500034140015, -47.42413220539094709 ) ) ;
#15529 = CARTESIAN_POINT ( 'NONE',  ( 0.000000000000000000, 22.50000000000000000, 102.0000000000000142 ) ) ;
#15530 = LINE ( 'NONE', #1888, #16433 ) ;
#15531 = CARTESIAN_POINT ( 'NONE',  ( -50.00000000000000000, 46.00000000000000000, 0.000000000000000000 ) ) ;
#15532 = PRESENTATION_STYLE_ASSIGNMENT (( #13050 ) ) ;
#15533 = DIRECTION ( 'NONE',  ( 0.000000000000000000, -0.000000000000000000, 1.000000000000000000 ) ) ;
#15534 = VECTOR ( 'NONE', #9860, 1000.000000000000000 ) ;
#15535 = CARTESIAN_POINT ( 'NONE',  ( 50.00000000000000000, 42.78125000068280315, -6.123233995736766085E-15 ) ) ;
#15536 = CARTESIAN_POINT ( 'NONE',  ( -15.45084971874736368, 38.18125000068280173, 47.55282581475768211 ) ) ;
#15537 = VECTOR ( 'NONE', #11636, 1000.000000000000114 ) ;
#15538 = DIRECTION ( 'NONE',  ( -0.000000000000000000, -1.000000000000000000, -0.000000000000000000 ) ) ;
#15539 = CARTESIAN_POINT ( 'NONE',  ( -9.500222237632405253, 22.00424054664139817, 101.0000000000000000 ) ) ;
#15540 = ADVANCED_FACE ( 'NONE', ( #15713 ), #7259, .T. ) ;
#15541 = ORIENTED_EDGE ( 'NONE', *, *, #13125, .F. ) ;
#15542 = CARTESIAN_POINT ( 'NONE',  ( -3.210462471511496205E-15, 35.35937500034140157, -52.43083105670540789 ) ) ;
#15543 = ORIENTED_EDGE ( 'NONE', *, *, #3052, .T. ) ;
#15544 = ORIENTED_EDGE ( 'NONE', *, *, #10785, .F. ) ;
#15545 = CARTESIAN_POINT ( 'NONE',  ( -3.219174618344376363E-15, 47.28125000068278894, -52.57311121191334990 ) ) ;
#15546 = AXIS2_PLACEMENT_3D ( 'NONE', #10221, #6576, #15274 ) ;
#15547 = CARTESIAN_POINT ( 'NONE',  ( -0.5000000000000000000, 39.99999999999999289, 101.0000000000000000 ) ) ;
#15548 = CARTESIAN_POINT ( 'NONE',  ( -40.34137639590981195, 20.05937500034139731, 29.30972558990012189 ) ) ;
#15549 = AXIS2_PLACEMENT_3D ( 'NONE', #2347, #1168, #11255 ) ;
#15550 = VERTEX_POINT ( 'NONE', #254 ) ;
#15551 = PRODUCT_DEFINITION_SHAPE ( 'NONE', 'NONE',  #2740 ) ;
#15552 = CYLINDRICAL_SURFACE ( 'NONE', #9735, 5.000000000000000000 ) ;
#15553 = CARTESIAN_POINT ( 'NONE',  ( 50.00000000000000000, 35.00000000000000000, -6.123233995736766085E-15 ) ) ;
#15554 = DIRECTION ( 'NONE',  ( 0.000000000000000000, 0.000000000000000000, 1.000000000000000000 ) ) ;
#15555 = CARTESIAN_POINT ( 'NONE',  ( -49.86468353124999453, 26.02187500034139589, 16.20201782572377169 ) ) ;
#15556 = EDGE_CURVE ( 'NONE', #798, #1879, #5669, .T. ) ;
#15557 = DIRECTION ( 'NONE',  ( 0.000000000000000000, 0.000000000000000000, 1.000000000000000000 ) ) ;
#15558 = VECTOR ( 'NONE', #14250, 1000.000000000000000 ) ;
#15559 = CARTESIAN_POINT ( 'NONE',  ( 9.341593500131070371, 7.690831593539996902, 98.20175713279056140 ) ) ;
#15560 = DIRECTION ( 'NONE',  ( 0.000000000000000000, 0.000000000000000000, 1.000000000000000000 ) ) ;
#15561 = CARTESIAN_POINT ( 'NONE',  ( 15.40903463028482356, 28.52187500034139589, 47.42413220539093999 ) ) ;
#15562 = DIRECTION ( 'NONE',  ( 0.000000000000000000, 1.000000000000000000, 0.000000000000000000 ) ) ;
#15563 = AXIS2_PLACEMENT_3D ( 'NONE', #16223, #14966, #15052 ) ;
#15564 = CARTESIAN_POINT ( 'NONE',  ( 50.00000000000000000, 35.00000000000000000, -6.123233995736766085E-15 ) ) ;
#15565 = CARTESIAN_POINT ( 'NONE',  ( -49.86468353124999453, 29.75937500034139305, -16.20201782572375393 ) ) ;
#15566 = CIRCLE ( 'NONE', #2288, 10.00000000000000355 ) ;
#15567 = VECTOR ( 'NONE', #6641, 1000.000000000000000 ) ;
#15568 = AXIS2_PLACEMENT_3D ( 'NONE', #12551, #2405, #7651 ) ;
#15569 = EDGE_CURVE ( 'NONE', #960, #7551, #10736, .T. ) ;
#15570 = CARTESIAN_POINT ( 'NONE',  ( 7.919222016226875382, 39.44874571845315359, -49.99999999999997158 ) ) ;
#15571 = ORIENTED_EDGE ( 'NONE', *, *, #13920, .F. ) ;
#15572 = EDGE_CURVE ( 'NONE', #75, #8799, #7828, .T. ) ;
#15573 = CARTESIAN_POINT ( 'NONE',  ( 49.86468353125001585, 26.75937500034139660, 16.20201782572375038 ) ) ;
#15574 = ORIENTED_EDGE ( 'NONE', *, *, #13561, .T. ) ;
#15575 = DIRECTION ( 'NONE',  ( 0.000000000000000000, 0.000000000000000000, 1.000000000000000000 ) ) ;
#15576 = CARTESIAN_POINT ( 'NONE',  ( 49.86468353125001585, 42.75937500034138594, 16.20201782572375038 ) ) ;
#15577 = LINE ( 'NONE', #7847, #4646 ) ;
#15578 = VECTOR ( 'NONE', #3309, 1000.000000000000000 ) ;
#15579 = CARTESIAN_POINT ( 'NONE',  ( 30.00000000000000000, 282.0000000000000000, 12.50000000000000178 ) ) ;
#15580 = VECTOR ( 'NONE', #79, 1000.000000000000000 ) ;
#15581 = CARTESIAN_POINT ( 'NONE',  ( -25.75618375337248978, 283.9316295015381115, 8.256183753373989020 ) ) ;
#15582 = CARTESIAN_POINT ( 'NONE',  ( 49.86468353125001585, 32.82187500034139305, 16.20201782572375038 ) ) ;
#15583 = CARTESIAN_POINT ( 'NONE',  ( 30.81806926056962936, 35.15937500034139873, -42.41743335407646498 ) ) ;
#15584 = FACE_OUTER_BOUND ( 'NONE', #1004, .T. ) ;
#15585 = CARTESIAN_POINT ( 'NONE',  ( 50.00000000000000000, 39.00000000000000000, -6.123233995736766085E-15 ) ) ;
#15586 = CARTESIAN_POINT ( 'NONE',  ( 49.86468353125001585, 48.75937500034140015, 16.20201782572375038 ) ) ;
#15587 = CARTESIAN_POINT ( 'NONE',  ( -15.40903463028481646, 43.52187500034139589, -47.42413220539093999 ) ) ;
#15588 = CARTESIAN_POINT ( 'NONE',  ( -49.86468353124999453, 25.82187500034139305, -16.20201782572375393 ) ) ;
#15589 = CONICAL_SURFACE ( 'NONE', #1785, 89.49773270518483059, 0.1745329251994333364 ) ;
#15590 = EDGE_CURVE ( 'NONE', #15550, #6081, #1511, .T. ) ;
#15592 =( BOUNDED_CURVE ( )  B_SPLINE_CURVE ( 2, ( #13813, #3848, #7586, #3931, #6431, #2425, #14060, #6266, #8913, #12664, #2676, #11337, #16404 ),
 .UNSPECIFIED., .F., .F. ) 
 B_SPLINE_CURVE_WITH_KNOTS ( ( 3, 2, 2, 2, 2, 2, 3 ),
 ( 0.6166666666666666963, 0.6199999999999999956, 0.6266666666666667052, 0.6333333333333333037, 0.6400000000000000133, 0.6466666666666666119, 0.6500000000000000222 ),
 .UNSPECIFIED. ) 
 CURVE ( )  GEOMETRIC_REPRESENTATION_ITEM ( )  RATIONAL_B_SPLINE_CURVE ( ( 0.9755282581475768211, 0.9755282581475771542, 1.000000000000000000, 0.9510565162951535312, 1.000000000000000000, 0.9510565162951535312, 1.000000000000000000, 0.9510565162951535312, 1.000000000000000000, 0.9510565162951535312, 1.000000000000000000, 0.9755282581475763770, 0.9755282581475768211 ) ) 
 REPRESENTATION_ITEM ( '' )  );
#15591 = VECTOR ( 'NONE', #9797, 1000.000000000000000 ) ;
#15593 = CARTESIAN_POINT ( 'NONE',  ( -30.90169943749473447, 28.08125000068280031, 42.53254041760200721 ) ) ;
#15594 = ORIENTED_EDGE ( 'NONE', *, *, #14886, .T. ) ;
#15595 = CARTESIAN_POINT ( 'NONE',  ( 40.45084971874737079, 30.98125000068279888, -29.38926261462366440 ) ) ;
#15596 = AXIS2_PLACEMENT_3D ( 'NONE', #16068, #7359, #15985 ) ;
#15597 = ORIENTED_EDGE ( 'NONE', *, *, #10903, .T. ) ;
#15598 = DIRECTION ( 'NONE',  ( 0.5000000000000041078, -0.8660254037844363761, -0.000000000000000000 ) ) ;
#15599 = CARTESIAN_POINT ( 'NONE',  ( 2.500000000000000000, 242.0000000000000284, 44.93050188902856945 ) ) ;
#15600 = CARTESIAN_POINT ( 'NONE',  ( 4.056709942754594067, 5.819547430268785959, 101.3333374614808662 ) ) ;
#15601 = CARTESIAN_POINT ( 'NONE',  ( -49.86468353124999453, 44.02187500034139589, 16.20201782572377169 ) ) ;
#15602 = CARTESIAN_POINT ( 'NONE',  ( -49.86468353124999453, 25.75937500034140015, -16.20201782572375393 ) ) ;
#15603 = DIRECTION ( 'NONE',  ( 0.000000000000000000, 0.000000000000000000, 1.000000000000000000 ) ) ;
#15604 = CARTESIAN_POINT ( 'NONE',  ( -15.40903463028481646, 39.52187500034139589, -47.42413220539093999 ) ) ;
#15605 = PRODUCT_CONTEXT ( 'NONE', #13844, 'mechanical' ) ;
#15606 = CARTESIAN_POINT ( 'NONE',  ( 3.465800365507340608, 94.69943522268255265, -5.000000000000000000 ) ) ;
#15607 = CARTESIAN_POINT ( 'NONE',  ( 15.40903463028482356, 44.52187500034139589, 47.42413220539093999 ) ) ;
#15608 = DIRECTION ( 'NONE',  ( -0.000000000000000000, -1.000000000000000000, -0.000000000000000000 ) ) ;
#15609 = ORIENTED_EDGE ( 'NONE', *, *, #8123, .F. ) ;
#15610 = CARTESIAN_POINT ( 'NONE',  ( 40.34137639590981195, 21.05937500034139376, -29.30972558990011834 ) ) ;
#15611 = ORIENTED_EDGE ( 'NONE', *, *, #15955, .T. ) ;
#15612 = CARTESIAN_POINT ( 'NONE',  ( -3.111920190527341144E-15, 45.28125000068279604, -50.00000000000000000 ) ) ;
#15613 = EDGE_LOOP ( 'NONE', ( #1915, #7033, #4043, #9113, #4149, #15783, #11283, #10851, #10446, #3958, #13371, #7883 ) ) ;
#15614 = CARTESIAN_POINT ( 'NONE',  ( -1.240322475938754499E-13, 36.50000000000000711, 50.00000000000000000 ) ) ;
#15615 = LINE ( 'NONE', #6742, #2106 ) ;
#15616 = CARTESIAN_POINT ( 'NONE',  ( 40.45084971874737789, 22.80000000000000071, 29.38926261462365375 ) ) ;
#15617 = CARTESIAN_POINT ( 'NONE',  ( 30.81806926056962936, 45.15937500034139873, -42.41743335407647209 ) ) ;
#15618 = CARTESIAN_POINT ( 'NONE',  ( 1.293669679204937499E-13, 37.28125000068280315, -50.00000000000000000 ) ) ;
#15619 = CARTESIAN_POINT ( 'NONE',  ( 0.5000000000000009992, 31.99999999999998579, 101.0000000000000000 ) ) ;
#15620 = CARTESIAN_POINT ( 'NONE',  ( 4.898587196589413026E-15, 267.0000000000000000, -40.00000000000000000 ) ) ;
#15621 = VECTOR ( 'NONE', #6142, 1000.000000000000227 ) ;
#15622 =( NAMED_UNIT ( * ) SI_UNIT ( $, .STERADIAN. ) SOLID_ANGLE_UNIT ( ) );
#15623 = CARTESIAN_POINT ( 'NONE',  ( 0.000000000000000000, 28.00000000000000355, 0.000000000000000000 ) ) ;
#15624 = CARTESIAN_POINT ( 'NONE',  ( -15.45084971874737256, 39.38125000068279746, -47.55282581475767500 ) ) ;
#15625 = CARTESIAN_POINT ( 'NONE',  ( -16.47405064338592595, 27.32701241865528985, 101.3333374614808662 ) ) ;
#15626 = CARTESIAN_POINT ( 'NONE',  ( 30.90169943749473802, 21.08125000068279675, -42.53254041760200721 ) ) ;
#15627 = DIRECTION ( 'NONE',  ( 0.000000000000000000, -1.000000000000000000, 0.000000000000000000 ) ) ;
#15628 = ORIENTED_EDGE ( 'NONE', *, *, #3788, .F. ) ;
#15629 = CARTESIAN_POINT ( 'NONE',  ( 40.34137639590981905, 36.65937500034139873, 29.30972558990010768 ) ) ;
#15630 = ORIENTED_EDGE ( 'NONE', *, *, #4081, .T. ) ;
#15631 = EDGE_LOOP ( 'NONE', ( #15436, #5296, #9857, #16205 ) ) ;
#15632 = DIRECTION ( 'NONE',  ( -0.000000000000000000, 1.000000000000000000, -0.000000000000000000 ) ) ;
#15633 = AXIS2_PLACEMENT_3D ( 'NONE', #11880, #314, #9232 ) ;
#15634 = CARTESIAN_POINT ( 'NONE',  ( 0.000000000000000000, 0.000000000000000000, 0.000000000000000000 ) ) ;
#15636 = CARTESIAN_POINT ( 'NONE',  ( -30.81806926056963292, 21.55937500034140086, -42.41743335407647209 ) ) ;
#15635 =( BOUNDED_CURVE ( )  B_SPLINE_CURVE ( 2, ( #63, #5090, #12879, #11394, #7482, #16459, #11467, #1316, #7563, #6240, #5169, #10065, #14037 ),
 .UNSPECIFIED., .F., .F. ) 
 B_SPLINE_CURVE_WITH_KNOTS ( ( 3, 2, 2, 2, 2, 2, 3 ),
 ( 0.5500000000000000444, 0.5533333333333333437, 0.5600000000000000533, 0.5666666666666666519, 0.5733333333333333615, 0.5799999999999999600, 0.5833333333333333703 ),
 .UNSPECIFIED. ) 
 CURVE ( )  GEOMETRIC_REPRESENTATION_ITEM ( )  RATIONAL_B_SPLINE_CURVE ( ( 0.9755282581475768211, 0.9755282581475771542, 1.000000000000000000, 0.9510565162951535312, 1.000000000000000000, 0.9510565162951535312, 1.000000000000000000, 0.9510565162951535312, 1.000000000000000000, 0.9510565162951535312, 1.000000000000000000, 0.9755282581475763770, 0.9755282581475768211 ) ) 
 REPRESENTATION_ITEM ( '' )  );
#15637 = ORIENTED_EDGE ( 'NONE', *, *, #6628, .T. ) ;
#15638 = PLANE ( 'NONE',  #1744 ) ;
#15639 = CARTESIAN_POINT ( 'NONE',  ( 7.919222016226809657, 35.44874571845314648, -50.00000000000000000 ) ) ;
#15640 = CARTESIAN_POINT ( 'NONE',  ( -4.127528389677584286, 5.486372832567261604, 102.0000000000000142 ) ) ;
#15641 = CARTESIAN_POINT ( 'NONE',  ( 40.34137639590981905, 30.72187500034139518, 29.30972558990010768 ) ) ;
#15642 = CARTESIAN_POINT ( 'NONE',  ( -40.45084971874737789, 37.58125000068280031, -29.38926261462365730 ) ) ;
#15643 = CYLINDRICAL_SURFACE ( 'NONE', #9659, 10.00000000000000000 ) ;
#15644 = DIRECTION ( 'NONE',  ( 0.000000000000000000, 1.000000000000000000, 0.000000000000000000 ) ) ;
#15645 = CARTESIAN_POINT ( 'NONE',  ( 40.34137639590981905, 28.72187500034139873, 29.30972558990010768 ) ) ;
#15646 = CARTESIAN_POINT ( 'NONE',  ( 3.078562342020788822, 5.611635739451020122, 101.3333374614808662 ) ) ;
#15647 = MECHANICAL_DESIGN_GEOMETRIC_PRESENTATION_REPRESENTATION (  '', ( #5827 ), #14049 ) ;
#15648 = CARTESIAN_POINT ( 'NONE',  ( -15.45084971874736368, 34.39999999999999858, 47.55282581475768211 ) ) ;
#15649 = CARTESIAN_POINT ( 'NONE',  ( 30.81806926056964002, 34.55937500034139731, 42.41743335407647209 ) ) ;
#15650 = DIRECTION ( 'NONE',  ( 0.000000000000000000, 0.000000000000000000, -1.000000000000000000 ) ) ;
#15651 = ORIENTED_EDGE ( 'NONE', *, *, #13724, .T. ) ;
#15652 = EDGE_CURVE ( 'NONE', #1083, #6085, #11656, .T. ) ;
#15653 = CARTESIAN_POINT ( 'NONE',  ( -3.210462471511496205E-15, 29.35937500034139802, -52.43083105670540789 ) ) ;
#15654 = ORIENTED_EDGE ( 'NONE', *, *, #15396, .F. ) ;
#15655 = PLANE ( 'NONE',  #6030 ) ;
#15656 = CARTESIAN_POINT ( 'NONE',  ( 49.86468353125001585, 44.75937500034138594, 16.20201782572375038 ) ) ;
#15657 = VECTOR ( 'NONE', #11789, 1000.000000000000000 ) ;
#15658 = DIRECTION ( 'NONE',  ( 1.000000000000000000, -6.145877457746401939E-15, 0.000000000000000000 ) ) ;
#15659 = CARTESIAN_POINT ( 'NONE',  ( 27.40717431545390781, 282.1599167565162816, 11.20358715772719371 ) ) ;
#15660 = EDGE_CURVE ( 'NONE', #9638, #2476, #9376, .T. ) ;
#15661 = EDGE_CURVE ( 'NONE', #9035, #8437, #14938, .T. ) ;
#15662 = CARTESIAN_POINT ( 'NONE',  ( -28.70358715772690061, 282.1599167565163384, 9.907174315453929125 ) ) ;
#15663 = CARTESIAN_POINT ( 'NONE',  ( 40.34137639590981905, 38.72187500034139873, 29.30972558990010768 ) ) ;
#15664 = CARTESIAN_POINT ( 'NONE',  ( -40.34137639590981905, 33.65937500034139873, -29.30972558990011478 ) ) ;
#15665 = DIRECTION ( 'NONE',  ( 6.938893903907231459E-18, -1.000000000000000000, -5.551115123125782702E-17 ) ) ;
#15666 = CARTESIAN_POINT ( 'NONE',  ( -15.45084971874737256, 43.60000000000000142, -47.55282581475767500 ) ) ;
#15667 = EDGE_CURVE ( 'NONE', #13340, #605, #9916, .T. ) ;
#15668 = CARTESIAN_POINT ( 'NONE',  ( -15.45084971874737256, 21.38125000068279746, -47.55282581475767500 ) ) ;
#15669 = CARTESIAN_POINT ( 'NONE',  ( -30.81806926056963292, 43.62187500034139020, -42.41743335407647209 ) ) ;
#15670 = CARTESIAN_POINT ( 'NONE',  ( 49.86468353125000164, 28.92187500034139802, -6.106662507704105588E-15 ) ) ;
#15671 = LINE ( 'NONE', #4294, #9415 ) ;
#15672 = VERTEX_POINT ( 'NONE', #5521 ) ;
#15673 = CARTESIAN_POINT ( 'NONE',  ( -30.90169943749474868, 31.48125000068279533, -42.53254041760200721 ) ) ;
#15674 = VERTEX_POINT ( 'NONE', #10824 ) ;
#15675 = DIRECTION ( 'NONE',  ( -0.000000000000000000, -1.000000000000000000, -0.000000000000000000 ) ) ;
#15676 = DIRECTION ( 'NONE',  ( 0.8660254037844513642, 0.4999999999999780731, 0.000000000000000000 ) ) ;
#15677 = CARTESIAN_POINT ( 'NONE',  ( 49.86468353124999453, 49.02187500034140299, -16.20201782572376104 ) ) ;
#15678 = CARTESIAN_POINT ( 'NONE',  ( -30.81806926056962226, 26.15937500034139163, 42.41743335407647919 ) ) ;
#15679 = CARTESIAN_POINT ( 'NONE',  ( 49.86468353124999453, 41.02187500034139589, -16.20201782572376104 ) ) ;
#15680 = DIRECTION ( 'NONE',  ( 0.000000000000000000, 0.000000000000000000, 1.000000000000000000 ) ) ;
#15681 = DIRECTION ( 'NONE',  ( 6.938893903907231459E-18, -1.000000000000000000, -5.551115123125782702E-17 ) ) ;
#15682 = CARTESIAN_POINT ( 'NONE',  ( 40.45084971874737789, 30.80000000000000071, 29.38926261462365375 ) ) ;
#15683 = ORIENTED_EDGE ( 'NONE', *, *, #16062, .F. ) ;
#15684 = CARTESIAN_POINT ( 'NONE',  ( 15.40903463028481113, 41.32187500034140015, -47.42413220539094709 ) ) ;
#15685 = PRODUCT_DEFINITION_SHAPE ( 'NONE', 'NONE',  #16467 ) ;
#15686 = ORIENTED_EDGE ( 'NONE', *, *, #590, .F. ) ;
#15687 = ORIENTED_EDGE ( 'NONE', *, *, #4003, .F. ) ;
#15688 = DIRECTION ( 'NONE',  ( -0.000000000000000000, -1.000000000000000000, -0.000000000000000000 ) ) ;
#15689 = CARTESIAN_POINT ( 'NONE',  ( 30.90169943749473802, 39.08125000068280031, -42.53254041760200721 ) ) ;
#15690 = DIRECTION ( 'NONE',  ( 0.000000000000000000, 0.000000000000000000, -1.000000000000000000 ) ) ;
#15691 = CARTESIAN_POINT ( 'NONE',  ( -15.45084971874736368, 26.40000000000000213, 47.55282581475768211 ) ) ;
#15692 = CARTESIAN_POINT ( 'NONE',  ( -49.86468353124999453, 43.95937500034138878, 16.20201782572377525 ) ) ;
#15693 = CARTESIAN_POINT ( 'NONE',  ( 7.919222016226822092, 48.33250428222964246, 49.99999999999999289 ) ) ;
#15694 = CARTESIAN_POINT ( 'NONE',  ( 0.000000000000000000, 50.00000000000000000, 0.000000000000000000 ) ) ;
#15695 = CARTESIAN_POINT ( 'NONE',  ( -49.99999999999999289, 46.09999999999999432, 16.24598481164533226 ) ) ;
#15696 = SHAPE_REPRESENTATION_RELATIONSHIP ( 'NONE' , 'NONE' ,  #10113, #8007 ) ;
#15697 = CARTESIAN_POINT ( 'NONE',  ( -10.29452708129647220, 9.181449853854553922, 101.6666710451724214 ) ) ;
#15698 = CARTESIAN_POINT ( 'NONE',  ( -40.45084971874737789, 35.58125000068279320, -29.38926261462365730 ) ) ;
#15699 = CARTESIAN_POINT ( 'NONE',  ( 0.000000000000000000, 50.00000000000000000, 0.000000000000000000 ) ) ;
#15700 = CARTESIAN_POINT ( 'NONE',  ( 30.90169943749473802, 23.08125000068279675, -42.53254041760200721 ) ) ;
#15701 = ADVANCED_FACE ( 'NONE', ( #9496 ), #14790, .T. ) ;
#15702 = FACE_BOUND ( 'NONE', #2340, .T. ) ;
#15703 = VERTEX_POINT ( 'NONE', #8556 ) ;
#15704 = CARTESIAN_POINT ( 'NONE',  ( -30.81806926056962226, 36.15937500034139163, 42.41743335407647919 ) ) ;
#15705 = ORIENTED_EDGE ( 'NONE', *, *, #13511, .F. ) ;
#15706 = ORIENTED_EDGE ( 'NONE', *, *, #14622, .F. ) ;
#15707 = DIRECTION ( 'NONE',  ( 0.000000000000000000, -1.000000000000000000, 0.000000000000000000 ) ) ;
#15708 = DIRECTION ( 'NONE',  ( 0.000000000000000000, 1.541976423090494894E-16, 1.000000000000000000 ) ) ;
#15709 = CARTESIAN_POINT ( 'NONE',  ( 30.81806926056964002, 22.55937500034139020, 42.41743335407647209 ) ) ;
#15710 = EDGE_LOOP ( 'NONE', ( #12866, #12273, #7071, #5907 ) ) ;
#15711 = CARTESIAN_POINT ( 'NONE',  ( -30.27664397204038593, 40.00000000000000711, 26.14048258526057467 ) ) ;
#15712 = CARTESIAN_POINT ( 'NONE',  ( 0.000000000000000000, 267.0000000000000000, 40.00000000000000000 ) ) ;
#15713 = FACE_OUTER_BOUND ( 'NONE', #11173, .T. ) ;
#15714 = CARTESIAN_POINT ( 'NONE',  ( 40.34137639590981195, 25.12187500034139376, -29.30972558990011834 ) ) ;
#15715 = DIRECTION ( 'NONE',  ( -0.000000000000000000, -1.000000000000000000, 0.000000000000000000 ) ) ;
#15716 = DIRECTION ( 'NONE',  ( -0.8660254037844399289, 0.000000000000000000, -0.4999999999999977796 ) ) ;
#15717 = CARTESIAN_POINT ( 'NONE',  ( -47.24032962522632317, 20.00000000000000355, 15.96451374291463310 ) ) ;
#15718 = CARTESIAN_POINT ( 'NONE',  ( -30.81806926056963292, 21.62187500034139376, -42.41743335407646498 ) ) ;
#15719 = CARTESIAN_POINT ( 'NONE',  ( 0.000000000000000000, 193.4213562373095385, 0.000000000000000000 ) ) ;
#15720 = CARTESIAN_POINT ( 'NONE',  ( 50.00000000000000711, 34.89999999999998437, 16.24598481164530739 ) ) ;
#15721 = CARTESIAN_POINT ( 'NONE',  ( -3.210462471511496205E-15, 35.35937500034140157, -52.43083105670540789 ) ) ;
#15722 = FACE_OUTER_BOUND ( 'NONE', #8866, .T. ) ;
#15723 = ORIENTED_EDGE ( 'NONE', *, *, #15048, .T. ) ;
#15724 =( BOUNDED_CURVE ( )  B_SPLINE_CURVE ( 2, ( #5679, #14799, #3433, #12155, #5930, #8494, #7175, #13558, #4439, #3514, #5848, #14553, #9586 ),
 .UNSPECIFIED., .F., .F. ) 
 B_SPLINE_CURVE_WITH_KNOTS ( ( 3, 2, 2, 2, 2, 2, 3 ),
 ( 0.6500000000000000222, 0.6533333333333333215, 0.6600000000000000311, 0.6666666666666666297, 0.6733333333333333393, 0.6800000000000000488, 0.6833333333333333481 ),
 .UNSPECIFIED. ) 
 CURVE ( )  GEOMETRIC_REPRESENTATION_ITEM ( )  RATIONAL_B_SPLINE_CURVE ( ( 0.9755282581475768211, 0.9755282581475771542, 1.000000000000000000, 0.9510565162951535312, 1.000000000000000000, 0.9510565162951535312, 1.000000000000000000, 0.9510565162951535312, 1.000000000000000000, 0.9510565162951535312, 1.000000000000000000, 0.9755282581475768211, 0.9755282581475768211 ) ) 
 REPRESENTATION_ITEM ( '' )  );
#15725 = CIRCLE ( 'NONE', #5401, 16.50000000000000711 ) ;
#15726 = CARTESIAN_POINT ( 'NONE',  ( 49.86468353124999453, 28.95937500034139589, -16.20201782572376104 ) ) ;
#15727 = VERTEX_POINT ( 'NONE', #15887 ) ;
#15728 = CARTESIAN_POINT ( 'NONE',  ( -3.111920190527341144E-15, 35.50000000000000000, -50.00000000000000000 ) ) ;
#15729 = CARTESIAN_POINT ( 'NONE',  ( 49.86468353125000164, 42.85937500034140157, -6.106662507704105588E-15 ) ) ;
#15730 = CARTESIAN_POINT ( 'NONE',  ( 24.76951992798502999, 286.3033656649012642, 7.269519927984441132 ) ) ;
#15731 = CARTESIAN_POINT ( 'NONE',  ( -26.78441608355137049, 282.9883952696293932, 9.284416083550581789 ) ) ;
#15732 = CARTESIAN_POINT ( 'NONE',  ( 49.86468353125001585, 38.82187500034140015, 16.20201782572375038 ) ) ;
#15733 = CARTESIAN_POINT ( 'NONE',  ( 49.86468353124999453, 36.95937500034139589, -16.20201782572376104 ) ) ;
#15734 = DIRECTION ( 'NONE',  ( 1.734723475976807094E-17, 0.000000000000000000, 1.000000000000000000 ) ) ;
#15735 = CARTESIAN_POINT ( 'NONE',  ( -30.81806926056962226, 30.22187500034139518, 42.41743335407647919 ) ) ;
#15736 = CARTESIAN_POINT ( 'NONE',  ( 15.45084971874737789, 40.60000000000000142, 47.55282581475767500 ) ) ;
#15737 = VECTOR ( 'NONE', #9755, 999.9999999999998863 ) ;
#15738 = EDGE_CURVE ( 'NONE', #2027, #15007, #14701, .T. ) ;
#15739 = CARTESIAN_POINT ( 'NONE',  ( -50.00000000000000000, 21.78125000068279959, 0.000000000000000000 ) ) ;
#15740 = CARTESIAN_POINT ( 'NONE',  ( -3.210462471511496205E-15, 41.42187500034140157, -52.43083105670540789 ) ) ;
#15741 = CARTESIAN_POINT ( 'NONE',  ( 9.631387414534489405E-15, 30.42187500034139447, 52.43083105670540789 ) ) ;
#15742 = EDGE_CURVE ( 'NONE', #3406, #3901, #9823, .T. ) ;
#15743 = EDGE_CURVE ( 'NONE', #14271, #9033, #5835, .T. ) ;
#15744 = CARTESIAN_POINT ( 'NONE',  ( 9.631387414534489405E-15, 46.35937500034139447, 52.43083105670540789 ) ) ;
#15745 = ORIENTED_EDGE ( 'NONE', *, *, #11930, .F. ) ;
#15746 = CARTESIAN_POINT ( 'NONE',  ( 30.90169943749475578, 30.48125000068279533, 42.53254041760200010 ) ) ;
#15747 = CIRCLE ( 'NONE', #3069, 45.00000000000000000 ) ;
#15748 = VERTEX_POINT ( 'NONE', #12054 ) ;
#15749 = ADVANCED_FACE ( 'NONE', ( #1988 ), #654, .F. ) ;
#15750 = CARTESIAN_POINT ( 'NONE',  ( 0.000000000000000000, 193.4213562373095385, 0.000000000000000000 ) ) ;
#15751 = CARTESIAN_POINT ( 'NONE',  ( 40.45084971874737789, 32.58125000068280031, 29.38926261462365375 ) ) ;
#15752 = CARTESIAN_POINT ( 'NONE',  ( 40.34137639590981905, 40.72187500034139873, 29.30972558990010768 ) ) ;
#15753 = CARTESIAN_POINT ( 'NONE',  ( 40.34137639590981905, 24.65937500034139873, 29.30972558990010768 ) ) ;
#15754 = LINE ( 'NONE', #3041, #7301 ) ;
#15755 = EDGE_CURVE ( 'NONE', #12890, #6301, #610, .T. ) ;
#15756 = APPLICATION_PROTOCOL_DEFINITION ( 'draft international standard', 'automotive_design', 1998, #14687 ) ;
#15757 = CARTESIAN_POINT ( 'NONE',  ( 50.00000000000000711, 34.89999999999998437, 16.24598481164530739 ) ) ;
#15758 = VECTOR ( 'NONE', #5673, 1000.000000000000000 ) ;
#15759 = VECTOR ( 'NONE', #7712, 1000.000000000000227 ) ;
#15760 = CARTESIAN_POINT ( 'NONE',  ( -49.86468353124999453, 49.82187500034140015, -16.20201782572375393 ) ) ;
#15761 = CARTESIAN_POINT ( 'NONE',  ( 2.600676159226420495E-13, 31.49999999999999289, -49.99999999999999289 ) ) ;
#15762 = ORIENTED_EDGE ( 'NONE', *, *, #12093, .F. ) ;
#15763 = CARTESIAN_POINT ( 'NONE',  ( -3.210462471511496205E-15, 41.42187500034140157, -52.43083105670540789 ) ) ;
#15764 = VERTEX_POINT ( 'NONE', #4584 ) ;
#15765 = ORIENTED_EDGE ( 'NONE', *, *, #15079, .T. ) ;
#15766 =( REPRESENTATION_RELATIONSHIP ('NONE','NONE', #6178, #10113 ) REPRESENTATION_RELATIONSHIP_WITH_TRANSFORMATION ( #4550 )SHAPE_REPRESENTATION_RELATIONSHIP( ) );
#15767 = ADVANCED_FACE ( 'NONE', ( #13550 ), #14159, .T. ) ;
#15768 = CYLINDRICAL_SURFACE ( 'NONE', #16391, 2.000000000000001776 ) ;
#15769 = DIRECTION ( 'NONE',  ( 0.000000000000000000, 1.000000000000000000, 0.000000000000000000 ) ) ;
#15770 = VECTOR ( 'NONE', #5377, 1000.000000000000227 ) ;
#15771 = CARTESIAN_POINT ( 'NONE',  ( 0.000000000000000000, 217.0000000000000284, 0.000000000000000000 ) ) ;
#15772 = CARTESIAN_POINT ( 'NONE',  ( 40.45084971874737079, 36.98125000068279888, -29.38926261462366440 ) ) ;
#15773 = CARTESIAN_POINT ( 'NONE',  ( -40.34137639590981905, 43.65937500034139163, -29.30972558990011478 ) ) ;
#15774 = DIRECTION ( 'NONE',  ( 0.9781476007338069101, -0.2079116908177532363, 0.000000000000000000 ) ) ;
#15775 = CARTESIAN_POINT ( 'NONE',  ( -8.660254037844387298, 25.00000000000000355, 5.000000000000000000 ) ) ;
#15776 = ADVANCED_FACE ( 'NONE', ( #13627 ), #11158, .F. ) ;
#15777 = CARTESIAN_POINT ( 'NONE',  ( -30.90169943749474513, 33.48125000068279888, -42.53254041760200721 ) ) ;
#15778 = SURFACE_SIDE_STYLE ('',( #10717 ) ) ;
#15779 = CARTESIAN_POINT ( 'NONE',  ( -49.93234176562499727, 49.96093750017070079, 0.000000000000000000 ) ) ;
#15780 = DIRECTION ( 'NONE',  ( 0.4999999999999977240, 0.000000000000000000, -0.8660254037844398178 ) ) ;
#15781 = DIRECTION ( 'NONE',  ( -0.000000000000000000, -0.7071067811865487940, -0.7071067811865463515 ) ) ;
#15782 = VECTOR ( 'NONE', #10625, 1000.000000000000000 ) ;
#15783 = ORIENTED_EDGE ( 'NONE', *, *, #5622, .F. ) ;
#15784 = CONICAL_SURFACE ( 'NONE', #1451, 16.50000000000000711, 0.7853981633974447263 ) ;
#15785 = CARTESIAN_POINT ( 'NONE',  ( -3.210462471511496205E-15, 29.35937500034139802, -52.43083105670540789 ) ) ;
#15786 = EDGE_LOOP ( 'NONE', ( #4181, #14259 ) ) ;
#15787 = ORIENTED_EDGE ( 'NONE', *, *, #7266, .T. ) ;
#15788 = ORIENTED_EDGE ( 'NONE', *, *, #11104, .F. ) ;
#15789 = ADVANCED_FACE ( 'NONE', ( #3421 ), #9649, .F. ) ;
#15790 = CARTESIAN_POINT ( 'NONE',  ( 15.45084971874737789, 48.38125000068280457, 47.55282581475767500 ) ) ;
#15791 = LINE ( 'NONE', #11972, #6298 ) ;
#15792 = CARTESIAN_POINT ( 'NONE',  ( -3.210462471511496205E-15, 21.35937500034139092, -52.43083105670540789 ) ) ;
#15793 = VERTEX_POINT ( 'NONE', #2078 ) ;
#15794 = CARTESIAN_POINT ( 'NONE',  ( -3.987376076617207499, 6.145737624504182151, 101.6666710451724214 ) ) ;
#15795 = DIRECTION ( 'NONE',  ( 1.000000000000000000, 0.000000000000000000, -0.000000000000000000 ) ) ;
#15796 = CARTESIAN_POINT ( 'NONE',  ( 0.000000000000000000, 22.50000000000000000, 102.0000000000000142 ) ) ;
#15797 = CARTESIAN_POINT ( 'NONE',  ( -15.40903463028480580, 28.32187500034139660, 47.42413220539094709 ) ) ;
#15798 = VECTOR ( 'NONE', #6140, 1000.000000000000000 ) ;
#15799 = CARTESIAN_POINT ( 'NONE',  ( 7.919222016226758143, 38.55125428154684641, 50.00000000000000711 ) ) ;
#15800 = CARTESIAN_POINT ( 'NONE',  ( 16.61632465174088580, 16.89218409470073468, 95.58913275680403387 ) ) ;
#15801 = CARTESIAN_POINT ( 'NONE',  ( -47.98103867763168040, 19.99999999999999645, 13.57697939761855643 ) ) ;
#15802 = CARTESIAN_POINT ( 'NONE',  ( -40.34137639590981195, 20.12187500034139731, 29.30972558990012189 ) ) ;
#15803 = CARTESIAN_POINT ( 'NONE',  ( -1.790468199911972924, 101.0808929720139702, -9.080892972013931086 ) ) ;
#15804 = CARTESIAN_POINT ( 'NONE',  ( -49.99999999999999289, 33.90000000000000568, -16.24598481164531449 ) ) ;
#15805 = CARTESIAN_POINT ( 'NONE',  ( -30.81806926056963292, 25.55937500034139376, -42.41743335407647209 ) ) ;
#15806 = CARTESIAN_POINT ( 'NONE',  ( -30.81806926056963292, 47.55937500034139731, -42.41743335407647209 ) ) ;
#15807 = EDGE_LOOP ( 'NONE', ( #4879, #5737, #5659, #15762 ) ) ;
#15808 = AXIS2_PLACEMENT_3D ( 'NONE', #6289, #7522, #14078 ) ;
#15809 = VECTOR ( 'NONE', #10087, 1000.000000000000000 ) ;
#15810 = CARTESIAN_POINT ( 'NONE',  ( -40.34137639590981905, 31.65937500034139873, -29.30972558990011478 ) ) ;
#15811 = ORIENTED_EDGE ( 'NONE', *, *, #7941, .T. ) ;
#15812 = AXIS2_PLACEMENT_3D ( 'NONE', #2158, #11073, #8560 ) ;
#15813 = DIRECTION ( 'NONE',  ( -0.9777979793268667397, -0.2095497831645171394, -0.000000000000000000 ) ) ;
#15814 = CARTESIAN_POINT ( 'NONE',  ( -3.210462471511496205E-15, 39.35937500034138736, -52.43083105670540789 ) ) ;
#15815 = ADVANCED_FACE ( 'NONE', ( #10979 ), #16043, .F. ) ;
#15816 = PLANE ( 'NONE',  #13090 ) ;
#15817 = CARTESIAN_POINT ( 'NONE',  ( -24.93825083352641769, 285.3724546740604637, 7.438250833527376926 ) ) ;
#15818 = CARTESIAN_POINT ( 'NONE',  ( -40.34137639590981905, 29.72187500034139518, -29.30972558990011478 ) ) ;
#15819 = CARTESIAN_POINT ( 'NONE',  ( -30.81806926056962226, 34.15937500034139163, 42.41743335407647209 ) ) ;
#15820 = AXIS2_PLACEMENT_3D ( 'NONE', #9858, #13667, #7373 ) ;
#15821 = AXIS2_PLACEMENT_3D ( 'NONE', #2421, #9841, #16063 ) ;
#15822 = CARTESIAN_POINT ( 'NONE',  ( -21.98588717320197006, 102.5902090043563533, -5.000000000000000000 ) ) ;
#15823 = CARTESIAN_POINT ( 'NONE',  ( 40.34137639590981195, 29.12187500034139376, -29.30972558990011834 ) ) ;
#15824 = CIRCLE ( 'NONE', #8657, 49.99999999999999289 ) ;
#15825 = CARTESIAN_POINT ( 'NONE',  ( 30.90169943749474157, 43.30000000000000426, -42.53254041760200721 ) ) ;
#15826 = CARTESIAN_POINT ( 'NONE',  ( -40.34137639590981195, 48.05937500034139731, 29.30972558990012189 ) ) ;
#15827 = CARTESIAN_POINT ( 'NONE',  ( -15.40903463028480580, 46.32187500034140015, 47.42413220539094709 ) ) ;
#15828 =( GEOMETRIC_REPRESENTATION_CONTEXT ( 3 ) GLOBAL_UNCERTAINTY_ASSIGNED_CONTEXT ( ( #10262 ) ) GLOBAL_UNIT_ASSIGNED_CONTEXT ( ( #1216, #49, #129 ) ) REPRESENTATION_CONTEXT ( 'NONE', 'WORKASPACE' ) );
#15829 = SHAPE_REPRESENTATION ( 'Rubber Leak-Proof Gasket Ring', ( #15812 ), #1738 ) ;
#15830 = CARTESIAN_POINT ( 'NONE',  ( 40.45084971874737789, 48.80000000000000426, 29.38926261462365375 ) ) ;
#15831 = EDGE_CURVE ( 'NONE', #5700, #14317, #7244, .T. ) ;
#15832 = EDGE_LOOP ( 'NONE', ( #10555, #7102 ) ) ;
#15833 = CARTESIAN_POINT ( 'NONE',  ( -49.86468353125000164, 49.85937500034139447, 0.000000000000000000 ) ) ;
#15834 = CIRCLE ( 'NONE', #15322, 5.000000000000000000 ) ;
#15835 = ORIENTED_EDGE ( 'NONE', *, *, #1971, .T. ) ;
#15836 = ORIENTED_EDGE ( 'NONE', *, *, #2183, .T. ) ;
#15837 = AXIS2_PLACEMENT_3D ( 'NONE', #9804, #14682, #13773 ) ;
#15839 = CARTESIAN_POINT ( 'NONE',  ( -40.45084971874737079, 31.98125000068280244, 29.38926261462367151 ) ) ;
#15838 = CIRCLE ( 'NONE', #12124, 40.00000000000000000 ) ;
#15840 = ORIENTED_EDGE ( 'NONE', *, *, #7249, .F. ) ;
#15841 = CARTESIAN_POINT ( 'NONE',  ( 40.45084971874737789, 44.58125000068280031, 29.38926261462365375 ) ) ;
#15842 = CARTESIAN_POINT ( 'NONE',  ( -16.48898053797772789, 28.38332565970911148, 101.0000000000000000 ) ) ;
#15843 = CARTESIAN_POINT ( 'NONE',  ( 15.45084971874737789, 30.38125000068280102, 47.55282581475767500 ) ) ;
#15844 = CARTESIAN_POINT ( 'NONE',  ( -49.86468353124999453, 40.02187500034139589, 16.20201782572377169 ) ) ;
#15845 = CARTESIAN_POINT ( 'NONE',  ( 40.34137639590981195, 47.12187500034140442, -29.30972558990011834 ) ) ;
#15846 = ADVANCED_FACE ( 'NONE', ( #3503 ), #12146, .F. ) ;
#15847 = DIRECTION ( 'NONE',  ( -1.000000000000000000, 0.000000000000000000, 0.000000000000000000 ) ) ;
#15848 = AXIS2_PLACEMENT_3D ( 'NONE', #15970, #6495, #12559 ) ;
#15849 = SHAPE_DEFINITION_REPRESENTATION ( #547, #9477 ) ;
#15850 = CARTESIAN_POINT ( 'NONE',  ( -40.45084971874737079, 40.20000000000000284, 29.38926261462367151 ) ) ;
#15851 = CONICAL_SURFACE ( 'NONE', #14780, 16.50000000000000711, 0.7853981633974447263 ) ;
#15852 = CARTESIAN_POINT ( 'NONE',  ( 49.86468353124999453, 41.02187500034139589, -16.20201782572376459 ) ) ;
#15853 = CARTESIAN_POINT ( 'NONE',  ( -15.45084971874737256, 45.38125000068279746, -47.55282581475767500 ) ) ;
#15854 = VERTEX_POINT ( 'NONE', #905 ) ;
#15855 = CARTESIAN_POINT ( 'NONE',  ( 40.34137639590981195, 41.12187500034139731, -29.30972558990011834 ) ) ;
#15856 = ORIENTED_EDGE ( 'NONE', *, *, #8445, .F. ) ;
#15857 = ORIENTED_EDGE ( 'NONE', *, *, #12924, .T. ) ;
#15858 = EDGE_CURVE ( 'NONE', #7640, #14690, #1943, .T. ) ;
#15859 = ORIENTED_EDGE ( 'NONE', *, *, #3634, .F. ) ;
#15860 = CARTESIAN_POINT ( 'NONE',  ( 1.293669679204937499E-13, 39.28125000068280315, -50.00000000000000000 ) ) ;
#15861 = CARTESIAN_POINT ( 'NONE',  ( 16.16503364901090123, 28.27806893495066021, 101.3333374614808662 ) ) ;
#15862 = CARTESIAN_POINT ( 'NONE',  ( 0.000000000000000000, 252.0000000000000000, 0.000000000000000000 ) ) ;
#15863 = DIRECTION ( 'NONE',  ( -6.938893903907231459E-18, 1.000000000000000000, 5.551115123125782702E-17 ) ) ;
#15864 = ADVANCED_FACE ( 'NONE', ( #4766 ), #16287, .T. ) ;
#15865 = CARTESIAN_POINT ( 'NONE',  ( -30.81806926056963292, 43.55937500034139731, -42.41743335407647209 ) ) ;
#15866 = CARTESIAN_POINT ( 'NONE',  ( -14.43699227201014423, 100.7369268407877456, 5.000000000000000000 ) ) ;
#15867 = CARTESIAN_POINT ( 'NONE',  ( 15.45084971874737789, 24.60000000000000142, 47.55282581475767500 ) ) ;
#15868 = DIRECTION ( 'NONE',  ( 1.000000000000000000, -0.000000000000000000, 1.224646799147353207E-16 ) ) ;
#15869 = CARTESIAN_POINT ( 'NONE',  ( 6.123233995736766085E-15, 20.00000000000000355, -50.00000000000000000 ) ) ;
#15870 = DIRECTION ( 'NONE',  ( -0.000000000000000000, -1.000000000000000000, -0.000000000000000000 ) ) ;
#15871 = EDGE_CURVE ( 'NONE', #1602, #16014, #7150, .T. ) ;
#15872 = CIRCLE ( 'NONE', #208, 47.00000000000000000 ) ;
#15873 = CARTESIAN_POINT ( 'NONE',  ( 7.513064459987437071E-14, 42.28125000068280315, 50.00000000000000000 ) ) ;
#15874 = DIRECTION ( 'NONE',  ( 0.000000000000000000, 0.000000000000000000, 1.000000000000000000 ) ) ;
#15875 = ORIENTED_EDGE ( 'NONE', *, *, #7282, .T. ) ;
#15876 = CARTESIAN_POINT ( 'NONE',  ( -40.34137639590981195, 34.05937500034139731, 29.30972558990012189 ) ) ;
#15877 = ORIENTED_EDGE ( 'NONE', *, *, #9667, .T. ) ;
#15878 = ORIENTED_EDGE ( 'NONE', *, *, #9988, .F. ) ;
#15879 = ORIENTED_EDGE ( 'NONE', *, *, #4962, .T. ) ;
#15880 = CARTESIAN_POINT ( 'NONE',  ( -30.90169943749473802, 46.08125000068278609, 42.53254041760200721 ) ) ;
#15881 = CARTESIAN_POINT ( 'NONE',  ( 9.189545401991395579, 24.96013318841451678, 102.0000000000000142 ) ) ;
#15882 = DIRECTION ( 'NONE',  ( 0.000000000000000000, 1.000000000000000000, 0.000000000000000000 ) ) ;
#15883 = EDGE_LOOP ( 'NONE', ( #9285, #7622 ) ) ;
#15884 = CARTESIAN_POINT ( 'NONE',  ( 0.000000000000000000, 22.50000000000000000, 100.0000000000000000 ) ) ;
#15885 = CARTESIAN_POINT ( 'NONE',  ( -50.00000000000000000, 48.00000000000000000, 0.000000000000000000 ) ) ;
#15886 = CARTESIAN_POINT ( 'NONE',  ( 0.000000000000000000, 279.6527036446661327, 0.000000000000000000 ) ) ;
#15887 = CARTESIAN_POINT ( 'NONE',  ( -45.11452830843730766, 20.00000000000000711, 21.24066852005664430 ) ) ;
#15888 = CARTESIAN_POINT ( 'NONE',  ( 9.631387414534489405E-15, 26.42187500034139447, 52.43083105670540789 ) ) ;
#15889 = CARTESIAN_POINT ( 'NONE',  ( 8.446640517145639571E-15, 48.49999999999999289, 50.00000000000000000 ) ) ;
#15890 = LINE ( 'NONE', #1992, #7275 ) ;
#15891 = CARTESIAN_POINT ( 'NONE',  ( 0.000000000000000000, 261.9999999999999432, 0.000000000000000000 ) ) ;
#15892 = ADVANCED_FACE ( 'NONE', ( #3670 ), #15042, .T. ) ;
#15893 = CARTESIAN_POINT ( 'NONE',  ( -40.34137639590981905, 21.72187500034139518, -29.30972558990011478 ) ) ;
#15894 = CARTESIAN_POINT ( 'NONE',  ( -41.80721665588497160, 98.34234248903787545, -5.000000000000000000 ) ) ;
#15895 = CARTESIAN_POINT ( 'NONE',  ( 9.657523855033129090E-15, 36.50000000000000711, 52.57311121191334990 ) ) ;
#15896 = CARTESIAN_POINT ( 'NONE',  ( -30.81806926056963292, 23.55937500034139376, -42.41743335407647209 ) ) ;
#15897 = CARTESIAN_POINT ( 'NONE',  ( -15.40903463028481646, 49.45937500034140299, -47.42413220539093999 ) ) ;
#15898 = VECTOR ( 'NONE', #16462, 1000.000000000000000 ) ;
#15899 = EDGE_LOOP ( 'NONE', ( #3568, #13699 ) ) ;
#15900 = UNCERTAINTY_MEASURE_WITH_UNIT (LENGTH_MEASURE( 1.000000000000000082E-05 ), #12392, 'distance_accuracy_value', 'NONE');
#15901 = CARTESIAN_POINT ( 'NONE',  ( 6.123233995736766085E-15, 193.4213562373095385, 50.00000000000000000 ) ) ;
#15902 = VERTEX_POINT ( 'NONE', #13792 ) ;
#15903 = CARTESIAN_POINT ( 'NONE',  ( -2.500000000000000000, 244.0000000000000284, 47.99999999999999289 ) ) ;
#15904 = CARTESIAN_POINT ( 'NONE',  ( 49.86468353125001585, 38.75937500034139305, 16.20201782572375038 ) ) ;
#15905 = CARTESIAN_POINT ( 'NONE',  ( 40.45084971874737079, 28.98125000068279888, -29.38926261462366440 ) ) ;
#15906 = FACE_OUTER_BOUND ( 'NONE', #8932, .T. ) ;
#15907 = CARTESIAN_POINT ( 'NONE',  ( 15.40903463028482356, 26.52187500034139589, 47.42413220539093999 ) ) ;
#15908 = CARTESIAN_POINT ( 'NONE',  ( 15.40903463028481113, 33.25937500034140015, -47.42413220539094709 ) ) ;
#15909 = CARTESIAN_POINT ( 'NONE',  ( -15.45084971874736368, 36.39999999999999858, 47.55282581475768211 ) ) ;
#15910 = CARTESIAN_POINT ( 'NONE',  ( 40.34137639590981905, 32.72187500034139873, 29.30972558990010768 ) ) ;
#15911 = DIRECTION ( 'NONE',  ( -0.000000000000000000, -1.000000000000000000, -0.000000000000000000 ) ) ;
#15912 = CARTESIAN_POINT ( 'NONE',  ( 40.34137639590981905, 42.65937500034139873, 29.30972558990010768 ) ) ;
#15913 = CARTESIAN_POINT ( 'NONE',  ( 30.81806926056962936, 47.22187500034139873, -42.41743335407647209 ) ) ;
#15914 = EDGE_CURVE ( 'NONE', #5468, #4312, #12637, .T. ) ;
#15915 = CARTESIAN_POINT ( 'NONE',  ( -15.40903463028481646, 21.52187500034139589, -47.42413220539093999 ) ) ;
#15916 = EDGE_CURVE ( 'NONE', #4820, #4055, #7652, .T. ) ;
#15917 = ORIENTED_EDGE ( 'NONE', *, *, #2914, .F. ) ;
#15918 = CARTESIAN_POINT ( 'NONE',  ( -49.86468353124999453, 49.75937500034137884, -16.20201782572375393 ) ) ;
#15919 = ORIENTED_EDGE ( 'NONE', *, *, #11624, .T. ) ;
#15920 = ORIENTED_EDGE ( 'NONE', *, *, #9277, .T. ) ;
#15921 = CARTESIAN_POINT ( 'NONE',  ( -40.45084971874737789, 33.58125000068280031, -29.38926261462365730 ) ) ;
#15922 = ORIENTED_EDGE ( 'NONE', *, *, #10109, .T. ) ;
#15923 = PLANE ( 'NONE',  #15281 ) ;
#15924 = CARTESIAN_POINT ( 'NONE',  ( 49.86468353125000164, 40.92187500034139447, -6.106662507704105588E-15 ) ) ;
#15925 = CARTESIAN_POINT ( 'NONE',  ( -49.86468353125000164, 45.92187500034139447, 0.000000000000000000 ) ) ;
#15926 = LINE ( 'NONE', #14501, #5189 ) ;
#15927 =( BOUNDED_CURVE ( )  B_SPLINE_CURVE ( 2, ( #15086, #3790, #7613, #11360, #12687, #8855, #1284, #12932, #7853, #2620, #7524, #4033, #6626 ),
 .UNSPECIFIED., .F., .F. ) 
 B_SPLINE_CURVE_WITH_KNOTS ( ( 3, 2, 2, 2, 2, 2, 3 ),
 ( 0.7833333333333333259, 0.7866666666666666252, 0.7933333333333333348, 0.8000000000000000444, 0.8066666666666666430, 0.8133333333333333526, 0.8166666666666666519 ),
 .UNSPECIFIED. ) 
 CURVE ( )  GEOMETRIC_REPRESENTATION_ITEM ( )  RATIONAL_B_SPLINE_CURVE ( ( 0.9755282581475768211, 0.9755282581475768211, 1.000000000000000000, 0.9510565162951535312, 1.000000000000000000, 0.9510565162951535312, 1.000000000000000000, 0.9510565162951535312, 1.000000000000000000, 0.9510565162951535312, 1.000000000000000000, 0.9755282581475768211, 0.9755282581475768211 ) ) 
 REPRESENTATION_ITEM ( '' )  );
#15928 = CARTESIAN_POINT ( 'NONE',  ( 9.631387414534489405E-15, 24.42187500034139447, 52.43083105670540789 ) ) ;
#15929 = CARTESIAN_POINT ( 'NONE',  ( 40.45084971874737079, 37.20000000000000284, -29.38926261462366440 ) ) ;
#15930 = CARTESIAN_POINT ( 'NONE',  ( 49.86468353125000164, 42.92187500034140157, -6.106662507704105588E-15 ) ) ;
#15931 = FACE_OUTER_BOUND ( 'NONE', #10056, .T. ) ;
#15932 = EDGE_LOOP ( 'NONE', ( #8175, #10650, #6716, #14714 ) ) ;
#15933 = CARTESIAN_POINT ( 'NONE',  ( -3.210462471511496205E-15, 39.42187500034140157, -52.43083105670540789 ) ) ;
#15934 = ORIENTED_EDGE ( 'NONE', *, *, #4622, .F. ) ;
#15935 = ORIENTED_EDGE ( 'NONE', *, *, #4107, .F. ) ;
#15936 = VERTEX_POINT ( 'NONE', #12721 ) ;
#15937 = DIRECTION ( 'NONE',  ( 6.938893903907231459E-18, -1.000000000000000000, -5.551115123125782702E-17 ) ) ;
#15938 = CARTESIAN_POINT ( 'NONE',  ( 12.41734070063129813, 34.35344015107605742, 101.3333374614808662 ) ) ;
#15939 = CARTESIAN_POINT ( 'NONE',  ( 4.391452393547104422E-14, 45.00000000000001421, 10.00000000000000355 ) ) ;
#15940 = CARTESIAN_POINT ( 'NONE',  ( -15.45084971874737256, 21.60000000000000142, -47.55282581475767500 ) ) ;
#15941 = CARTESIAN_POINT ( 'NONE',  ( 30.81806926056962936, 39.15937500034139873, -42.41743335407647209 ) ) ;
#15942 = CARTESIAN_POINT ( 'NONE',  ( -40.34137639590981195, 48.05937500034139731, 29.30972558990012189 ) ) ;
#15943 = CARTESIAN_POINT ( 'NONE',  ( 17.28626291527370284, 40.00000000000000711, -18.64048258526063151 ) ) ;
#15944 = DIRECTION ( 'NONE',  ( -0.000000000000000000, -1.000000000000000000, -0.000000000000000000 ) ) ;
#15945 =( NAMED_UNIT ( * ) SI_UNIT ( $, .STERADIAN. ) SOLID_ANGLE_UNIT ( ) );
#15946 = DIRECTION ( 'NONE',  ( 0.000000000000000000, 0.000000000000000000, 1.000000000000000000 ) ) ;
#15947 = EDGE_CURVE ( 'NONE', #10158, #11932, #8807, .T. ) ;
#15948 = CARTESIAN_POINT ( 'NONE',  ( 7.919222016226875382, 41.44874571845315359, -49.99999999999997158 ) ) ;
#15949 = CARTESIAN_POINT ( 'NONE',  ( 0.000000000000000000, 261.9999999999999432, 0.000000000000000000 ) ) ;
#15950 = ORIENTED_EDGE ( 'NONE', *, *, #15379, .T. ) ;
#15951 = CARTESIAN_POINT ( 'NONE',  ( 49.86468353125000164, 30.85937500034139802, -6.106662507704105588E-15 ) ) ;
#15952 = VERTEX_POINT ( 'NONE', #8980 ) ;
#15953 = VERTEX_POINT ( 'NONE', #9902 ) ;
#15954 = VERTEX_POINT ( 'NONE', #16380 ) ;
#15955 = EDGE_CURVE ( 'NONE', #6571, #14589, #5015, .T. ) ;
#15956 = CARTESIAN_POINT ( 'NONE',  ( -15.45084971874737256, 45.38125000068279746, -47.55282581475767500 ) ) ;
#15957 = CARTESIAN_POINT ( 'NONE',  ( -7.919222016226752814, 39.55125428154683931, -50.00000000000000711 ) ) ;
#15958 = CARTESIAN_POINT ( 'NONE',  ( 50.00000000000000000, 29.00000000000000000, -6.123233995736766085E-15 ) ) ;
#15959 = EDGE_LOOP ( 'NONE', ( #13200, #12087, #8717 ) ) ;
#15960 = CARTESIAN_POINT ( 'NONE',  ( -49.99999999999999289, 27.88125000068280102, 16.24598481164533226 ) ) ;
#15961 = ADVANCED_FACE ( 'NONE', ( #6408 ), #8892, .F. ) ;
#15962 = CARTESIAN_POINT ( 'NONE',  ( -25.00000000000000355, 312.0000000000000568, 7.500000000000001776 ) ) ;
#15963 = DIRECTION ( 'NONE',  ( 0.000000000000000000, 0.000000000000000000, 1.000000000000000000 ) ) ;
#15964 = DIRECTION ( 'NONE',  ( 0.000000000000000000, 0.000000000000000000, 1.000000000000000000 ) ) ;
#15965 = CARTESIAN_POINT ( 'NONE',  ( 5.510910596163089556E-15, 242.0000000000000284, -45.00000000000000000 ) ) ;
#15966 = CARTESIAN_POINT ( 'NONE',  ( -2.547328955960238000E-13, 20.28125000068279959, 49.99999999999999289 ) ) ;
#15967 = CARTESIAN_POINT ( 'NONE',  ( -9.395693774364753281, 21.00971865127312199, 101.0000000000000000 ) ) ;
#15968 = LINE ( 'NONE', #8321, #11709 ) ;
#15969 = CARTESIAN_POINT ( 'NONE',  ( -15.40903463028481646, 21.52187500034139589, -47.42413220539093999 ) ) ;
#15970 = CARTESIAN_POINT ( 'NONE',  ( 7.574663982647604321, 38.28367718720770796, 101.0000000000000000 ) ) ;
#15971 = ADVANCED_FACE ( 'NONE', ( #6332 ), #872, .T. ) ;
#15972 = CARTESIAN_POINT ( 'NONE',  ( -15.45084971874737256, 27.60000000000000142, -47.55282581475767500 ) ) ;
#15973 = CARTESIAN_POINT ( 'NONE',  ( 49.86468353124999453, 28.95937500034139944, -16.20201782572376459 ) ) ;
#15974 = CARTESIAN_POINT ( 'NONE',  ( 49.86468353125000164, 48.85937500034139447, -6.106662507704105588E-15 ) ) ;
#15975 = ORIENTED_EDGE ( 'NONE', *, *, #5840, .F. ) ;
#15976 = CARTESIAN_POINT ( 'NONE',  ( 43.10890719796073256, 25.03031439394993640, -25.50054622961014061 ) ) ;
#15977 = ORIENTED_EDGE ( 'NONE', *, *, #5460, .T. ) ;
#15978 = DIRECTION ( 'NONE',  ( -1.000000000000000000, 0.000000000000000000, 0.000000000000000000 ) ) ;
#15979 = CARTESIAN_POINT ( 'NONE',  ( -30.81806926056963292, 33.55937500034138310, -42.41743335407647209 ) ) ;
#15980 = DIRECTION ( 'NONE',  ( -5.069245582283711292E-17, -1.000000000000000000, 8.780190904559502465E-17 ) ) ;
#15981 = CARTESIAN_POINT ( 'NONE',  ( 20.00000000000113332, 286.6727470533786573, 7.500000000000000888 ) ) ;
#15982 = CARTESIAN_POINT ( 'NONE',  ( 6.123233995736766085E-15, 20.00000000000000355, -50.00000000000000000 ) ) ;
#15983 = CARTESIAN_POINT ( 'NONE',  ( -15.40903463028481646, 29.52187500034139589, -47.42413220539093999 ) ) ;
#15984 = CARTESIAN_POINT ( 'NONE',  ( 40.34137639590981905, 28.65937500034139873, 29.30972558990010768 ) ) ;
#15985 = DIRECTION ( 'NONE',  ( 0.000000000000000000, 0.000000000000000000, 1.000000000000000000 ) ) ;
#15986 = CARTESIAN_POINT ( 'NONE',  ( -40.34137639590981195, 30.12187500034139731, 29.30972558990012189 ) ) ;
#15987 = ADVANCED_FACE ( 'NONE', ( #15283 ), #7729, .F. ) ;
#15988 = PLANE ( 'NONE',  #8935 ) ;
#15989 = CARTESIAN_POINT ( 'NONE',  ( 49.86468353124999453, 46.95937500034139589, -16.20201782572376459 ) ) ;
#15990 = CARTESIAN_POINT ( 'NONE',  ( 40.34137639590981195, 35.12187500034139731, -29.30972558990011834 ) ) ;
#15991 = AXIS2_PLACEMENT_3D ( 'NONE', #6984, #10811, #15874 ) ;
#15992 = CARTESIAN_POINT ( 'NONE',  ( -30.81806926056962226, 20.22187500034139163, 42.41743335407647919 ) ) ;
#15993 = VERTEX_POINT ( 'NONE', #3912 ) ;
#15994 = CARTESIAN_POINT ( 'NONE',  ( -49.86468353124999453, 39.75937500034139305, -16.20201782572375393 ) ) ;
#15995 = EDGE_LOOP ( 'NONE', ( #7539, #14293, #52, #3919 ) ) ;
#15996 = CARTESIAN_POINT ( 'NONE',  ( 50.00000000000000711, 22.68125000068279462, 16.24598481164530739 ) ) ;
#15997 = ORIENTED_EDGE ( 'NONE', *, *, #16301, .T. ) ;
#15998 = VECTOR ( 'NONE', #12191, 1000.000000000000000 ) ;
#15999 = CARTESIAN_POINT ( 'NONE',  ( -15.45084971874737256, 33.38125000068280457, -47.55282581475767500 ) ) ;
#16000 = CARTESIAN_POINT ( 'NONE',  ( 15.40903463028481113, 41.32187500034140015, -47.42413220539094709 ) ) ;
#16001 = EDGE_CURVE ( 'NONE', #7138, #14296, #3299, .T. ) ;
#16002 = CARTESIAN_POINT ( 'NONE',  ( -40.34137639590981905, 45.72187500034139873, -29.30972558990011478 ) ) ;
#16003 = FACE_OUTER_BOUND ( 'NONE', #9855, .T. ) ;
#16004 = CARTESIAN_POINT ( 'NONE',  ( 15.40903463028482356, 26.52187500034139589, 47.42413220539093999 ) ) ;
#16005 = APPLICATION_PROTOCOL_DEFINITION ( 'draft international standard', 'automotive_design', 1998, #14070 ) ;
#16006 = CARTESIAN_POINT ( 'NONE',  ( 30.90169943749474157, 37.08125000068279320, -42.53254041760200721 ) ) ;
#16007 = CARTESIAN_POINT ( 'NONE',  ( -15.45084971874736368, 38.40000000000000568, 47.55282581475768211 ) ) ;
#16008 = CARTESIAN_POINT ( 'NONE',  ( -30.81806926056962226, 38.22187500034139873, 42.41743335407647919 ) ) ;
#16009 = CARTESIAN_POINT ( 'NONE',  ( 50.00000000000000711, 30.89999999999999858, 16.24598481164530739 ) ) ;
#16010 = ORIENTED_EDGE ( 'NONE', *, *, #11387, .T. ) ;
#16011 = CARTESIAN_POINT ( 'NONE',  ( 49.86468353125001585, 42.82187500034139305, 16.20201782572375038 ) ) ;
#16012 = CARTESIAN_POINT ( 'NONE',  ( -7.919222016226688865, 31.33250428222963890, -50.00000000000003553 ) ) ;
#16013 = ORIENTED_EDGE ( 'NONE', *, *, #12809, .T. ) ;
#16014 = VERTEX_POINT ( 'NONE', #11235 ) ;
#16015 = ORIENTED_EDGE ( 'NONE', *, *, #6562, .T. ) ;
#16016 = CARTESIAN_POINT ( 'NONE',  ( 9.574901606694759531E-15, 52.00000000000001421, -2.191293403013901163E-14 ) ) ;
#16017 = DIRECTION ( 'NONE',  ( -0.000000000000000000, -1.000000000000000000, -0.000000000000000000 ) ) ;
#16018 =( BOUNDED_CURVE ( )  B_SPLINE_CURVE ( 2, ( #15098, #10292, #5235, #15345, #11371, #11212, #16437, #15175, #5071, #8702, #10124, #3803, #8867 ),
 .UNSPECIFIED., .F., .F. ) 
 B_SPLINE_CURVE_WITH_KNOTS ( ( 3, 2, 2, 2, 2, 2, 3 ),
 ( 0.1499999999999999944, 0.1533333333333333215, 0.1600000000000000033, 0.1666666666666666574, 0.1733333333333333393, 0.1799999999999999933, 0.1833333333333333481 ),
 .UNSPECIFIED. ) 
 CURVE ( )  GEOMETRIC_REPRESENTATION_ITEM ( )  RATIONAL_B_SPLINE_CURVE ( ( 0.9755282581475768211, 0.9755282581475768211, 1.000000000000000000, 0.9510565162951535312, 1.000000000000000000, 0.9510565162951535312, 1.000000000000000000, 0.9510565162951535312, 1.000000000000000000, 0.9510565162951535312, 1.000000000000000000, 0.9755282581475765991, 0.9755282581475767101 ) ) 
 REPRESENTATION_ITEM ( '' )  );
#16019 = CARTESIAN_POINT ( 'NONE',  ( 40.45084971874737079, 27.20000000000000284, -29.38926261462366440 ) ) ;
#16020 = CARTESIAN_POINT ( 'NONE',  ( 5.000000000000000000, 100.8332763660827567, 11.66170349082890212 ) ) ;
#16021 = CARTESIAN_POINT ( 'NONE',  ( 9.631387414534489405E-15, 40.35937500034139447, 52.43083105670540789 ) ) ;
#16022 = CARTESIAN_POINT ( 'NONE',  ( -40.34137639590981905, 49.65937500034139873, -29.30972558990011478 ) ) ;
#16023 = CARTESIAN_POINT ( 'NONE',  ( 40.45084971874737789, 24.80000000000000426, 29.38926261462365375 ) ) ;
#16024 = CARTESIAN_POINT ( 'NONE',  ( 14.03285685708579145, 13.82077604687259154, 102.0000000000000142 ) ) ;
#16025 = LINE ( 'NONE', #14771, #6776 ) ;
#16026 = CARTESIAN_POINT ( 'NONE',  ( 12.67046914267482016, 34.58135802401886139, 101.0000000000000000 ) ) ;
#16027 = CARTESIAN_POINT ( 'NONE',  ( 30.90169943749475223, 40.69999999999999574, 42.53254041760199300 ) ) ;
#16028 = CARTESIAN_POINT ( 'NONE',  ( -7.499999999999998224, 25.00000000000000355, -24.29058411375428150 ) ) ;
#16029 = EDGE_LOOP ( 'NONE', ( #1103, #4777 ) ) ;
#16030 = EDGE_CURVE ( 'NONE', #6698, #11148, #8326, .T. ) ;
#16031 = CARTESIAN_POINT ( 'NONE',  ( -30.81806926056962226, 32.15937500034139873, 42.41743335407647919 ) ) ;
#16032 = EDGE_CURVE ( 'NONE', #2741, #6400, #4377, .T. ) ;
#16033 = ORIENTED_EDGE ( 'NONE', *, *, #1009, .F. ) ;
#16034 = ORIENTED_EDGE ( 'NONE', *, *, #12294, .T. ) ;
#16035 = ORIENTED_EDGE ( 'NONE', *, *, #14923, .T. ) ;
#16036 = CARTESIAN_POINT ( 'NONE',  ( -49.99999999999999289, 41.68125000068280173, -16.24598481164531449 ) ) ;
#16037 = CARTESIAN_POINT ( 'NONE',  ( 10.09851121871635904, 9.451242543235769844, 102.0000000000000142 ) ) ;
#16038 = CARTESIAN_POINT ( 'NONE',  ( 50.00000000000000711, 28.89999999999999858, 16.24598481164530739 ) ) ;
#16039 = ORIENTED_EDGE ( 'NONE', *, *, #5916, .F. ) ;
#16040 = CARTESIAN_POINT ( 'NONE',  ( 0.000000000000000000, 272.0000000000000000, 0.000000000000000000 ) ) ;
#16041 = PLANE ( 'NONE',  #6813 ) ;
#16042 = DIRECTION ( 'NONE',  ( -0.000000000000000000, -1.000000000000000000, -0.000000000000000000 ) ) ;
#16043 = CYLINDRICAL_SURFACE ( 'NONE', #12840, 47.00000000000000000 ) ;
#16044 = FACE_OUTER_BOUND ( 'NONE', #3121, .T. ) ;
#16045 = CARTESIAN_POINT ( 'NONE',  ( 2.600676159226420495E-13, 31.49999999999999289, -49.99999999999999289 ) ) ;
#16046 =( NAMED_UNIT ( * ) PLANE_ANGLE_UNIT ( ) SI_UNIT ( $, .RADIAN. ) );
#16047 = ADVANCED_FACE ( 'NONE', ( #14198 ), #2980, .F. ) ;
#16048 = CARTESIAN_POINT ( 'NONE',  ( -45.25922935877468944, 20.00000000000001776, 20.93126818148126489 ) ) ;
#16049 = CARTESIAN_POINT ( 'NONE',  ( -30.81806926056962226, 20.22187500034139518, 42.41743335407647209 ) ) ;
#16050 = CARTESIAN_POINT ( 'NONE',  ( -3.149380788943775933, 5.278461141749506425, 101.0000000000000000 ) ) ;
#16051 = VECTOR ( 'NONE', #2322, 1000.000000000000000 ) ;
#16052 = CARTESIAN_POINT ( 'NONE',  ( -50.00000000000000000, 26.00000000000000355, 0.000000000000000000 ) ) ;
#16053 = CARTESIAN_POINT ( 'NONE',  ( 49.86468353125001585, 26.75937500034139660, 16.20201782572375038 ) ) ;
#16054 = CARTESIAN_POINT ( 'NONE',  ( -49.99999999999999289, 41.68125000068280173, -16.24598481164531449 ) ) ;
#16055 = CARTESIAN_POINT ( 'NONE',  ( 5.179451399591075145, 14.52044592729181538, 101.0000000000000000 ) ) ;
#16056 = ORIENTED_EDGE ( 'NONE', *, *, #10694, .T. ) ;
#16057 = CARTESIAN_POINT ( 'NONE',  ( -49.86468353125000164, 25.85937500034139802, 0.000000000000000000 ) ) ;
#16058 = VERTEX_POINT ( 'NONE', #13208 ) ;
#16059 = CARTESIAN_POINT ( 'NONE',  ( 5.510910596163089556E-15, 257.0000000000001137, -45.00000000000000000 ) ) ;
#16060 = CARTESIAN_POINT ( 'NONE',  ( -3.210462471511496205E-15, 35.35937500034140157, -52.43083105670540789 ) ) ;
#16061 = MECHANICAL_DESIGN_GEOMETRIC_PRESENTATION_REPRESENTATION (  '', ( #15256 ), #642 ) ;
#16062 = EDGE_CURVE ( 'NONE', #15993, #4476, #8836, .T. ) ;
#16063 = DIRECTION ( 'NONE',  ( 0.000000000000000000, 0.000000000000000000, 1.000000000000000000 ) ) ;
#16064 = CARTESIAN_POINT ( 'NONE',  ( 0.000000000000000000, 262.0000000000000000, 0.000000000000000000 ) ) ;
#16065 = CARTESIAN_POINT ( 'NONE',  ( 9.366734789577542680E-15, 82.00000000000001421, -2.024759949320127682E-14 ) ) ;
#16066 = CARTESIAN_POINT ( 'NONE',  ( 9.631387414534489405E-15, 28.42187500034139092, 52.43083105670540789 ) ) ;
#16067 = CARTESIAN_POINT ( 'NONE',  ( -40.34137639590981905, 27.65937500034139873, -29.30972558990011478 ) ) ;
#16068 = CARTESIAN_POINT ( 'NONE',  ( 0.000000000000000000, 52.26146722824297797, 0.000000000000000000 ) ) ;
#16069 = CARTESIAN_POINT ( 'NONE',  ( 30.81806926056964002, 30.62187500034139020, 42.41743335407647209 ) ) ;
#16070 = FACE_OUTER_BOUND ( 'NONE', #15078, .T. ) ;
#16071 = ADVANCED_FACE ( 'NONE', ( #9310 ), #10314, .F. ) ;
#16072 = CARTESIAN_POINT ( 'NONE',  ( -49.86468353124999453, 47.95937500034138878, 16.20201782572377525 ) ) ;
#16073 = CARTESIAN_POINT ( 'NONE',  ( -40.34137639590981905, 37.72187500034139873, -29.30972558990011478 ) ) ;
#16074 = CIRCLE ( 'NONE', #9967, 45.00000000000000000 ) ;
#16075 = EDGE_CURVE ( 'NONE', #10305, #8817, #4624, .T. ) ;
#16076 = CARTESIAN_POINT ( 'NONE',  ( 30.81806926056962936, 21.22187500034139518, -42.41743335407647209 ) ) ;
#16077 =( GEOMETRIC_REPRESENTATION_CONTEXT ( 3 ) GLOBAL_UNCERTAINTY_ASSIGNED_CONTEXT ( ( #4601 ) ) GLOBAL_UNIT_ASSIGNED_CONTEXT ( ( #8405, #16046, #3426 ) ) REPRESENTATION_CONTEXT ( 'NONE', 'WORKASPACE' ) );
#16078 = VERTEX_POINT ( 'NONE', #235 ) ;
#16079 = CARTESIAN_POINT ( 'NONE',  ( -30.81806926056962226, 44.15937500034139163, 42.41743335407647209 ) ) ;
#16080 = ORIENTED_EDGE ( 'NONE', *, *, #6710, .T. ) ;
#16081 = CARTESIAN_POINT ( 'NONE',  ( -50.00000000000000000, 25.78125000068279959, 0.000000000000000000 ) ) ;
#16082 = ORIENTED_EDGE ( 'NONE', *, *, #10903, .F. ) ;
#16083 = VECTOR ( 'NONE', #537, 1000.000000000000114 ) ;
#16084 = AXIS2_PLACEMENT_3D ( 'NONE', #10004, #3438, #3349 ) ;
#16085 = VECTOR ( 'NONE', #15468, 1000.000000000000000 ) ;
#16086 = AXIS2_PLACEMENT_3D ( 'NONE', #13713, #10372, #12481 ) ;
#16087 = CARTESIAN_POINT ( 'NONE',  ( -49.99999999999999289, 35.89999999999999858, -16.24598481164531449 ) ) ;
#16088 = CARTESIAN_POINT ( 'NONE',  ( 40.34137639590981195, 39.12187500034139731, -29.30972558990011834 ) ) ;
#16089 = CARTESIAN_POINT ( 'NONE',  ( -40.34137639590981195, 48.12187500034139731, 29.30972558990012189 ) ) ;
#16090 = APPLICATION_CONTEXT ( 'automotive_design' ) ;
#16091 = AXIS2_PLACEMENT_3D ( 'NONE', #10454, #9121, #2967 ) ;
#16092 = CARTESIAN_POINT ( 'NONE',  ( 40.45084971874737079, 41.20000000000000284, -29.38926261462366440 ) ) ;
#16093 = CARTESIAN_POINT ( 'NONE',  ( 49.86468353125000164, 26.92187500034139802, -6.106662507704105588E-15 ) ) ;
#16094 = CARTESIAN_POINT ( 'NONE',  ( -49.99999999999999289, 35.88125000068279746, 16.24598481164533226 ) ) ;
#16095 = EDGE_CURVE ( 'NONE', #4375, #8209, #5947, .T. ) ;
#16096 = CARTESIAN_POINT ( 'NONE',  ( -49.86468353125000164, 39.92187500034139447, 0.000000000000000000 ) ) ;
#16097 = AXIS2_PLACEMENT_3D ( 'NONE', #7572, #1246, #11169 ) ;
#16098 = CARTESIAN_POINT ( 'NONE',  ( -28.38892170791837799, 282.2553694771631854, -9.277843415833588736 ) ) ;
#16099 = CIRCLE ( 'NONE', #9469, 2.267949192431125027 ) ;
#16100 = CIRCLE ( 'NONE', #13703, 2.000000000000001776 ) ;
#16101 = ORIENTED_EDGE ( 'NONE', *, *, #4203, .F. ) ;
#16102 = CARTESIAN_POINT ( 'NONE',  ( 30.81806926056964002, 36.62187500034139731, 42.41743335407647209 ) ) ;
#16103 = CARTESIAN_POINT ( 'NONE',  ( -15.45084971874736368, 44.18125000068280173, 47.55282581475768211 ) ) ;
#16104 = ORIENTED_EDGE ( 'NONE', *, *, #15556, .T. ) ;
#16105 = ORIENTED_EDGE ( 'NONE', *, *, #6712, .T. ) ;
#16106 = ORIENTED_EDGE ( 'NONE', *, *, #7347, .F. ) ;
#16107 = PLANE ( 'NONE',  #4191 ) ;
#16108 = CARTESIAN_POINT ( 'NONE',  ( -50.00000000000000000, 50.00000000000000000, 0.000000000000000000 ) ) ;
#16109 = CARTESIAN_POINT ( 'NONE',  ( 40.45084971874737789, 36.58125000068280031, 29.38926261462365375 ) ) ;
#16110 = AXIS2_PLACEMENT_3D ( 'NONE', #5042, #2600, #1176 ) ;
#16111 = CARTESIAN_POINT ( 'NONE',  ( -40.34137639590981905, 37.65937500034139873, -29.30972558990011478 ) ) ;
#16112 = CIRCLE ( 'NONE', #11080, 5.000000000000000000 ) ;
#16113 = CARTESIAN_POINT ( 'NONE',  ( 49.86468353124999453, 48.95937500034140299, -16.20201782572376104 ) ) ;
#16114 = EDGE_CURVE ( 'NONE', #15191, #40, #16262, .T. ) ;
#16115 = CARTESIAN_POINT ( 'NONE',  ( -0.4999999999999990563, 31.99999999999998579, 102.0000000000000142 ) ) ;
#16116 = AXIS2_PLACEMENT_3D ( 'NONE', #11728, #2996, #8157 ) ;
#16117 = ADVANCED_FACE ( 'NONE', ( #11792 ), #13122, .F. ) ;
#16118 = SURFACE_STYLE_FILL_AREA ( #7311 ) ;
#16119 = CYLINDRICAL_SURFACE ( 'NONE', #1950, 42.00000000000000711 ) ;
#16120 = DIRECTION ( 'NONE',  ( 0.4067366430758010964, -0.9135454576426004225, 0.000000000000000000 ) ) ;
#16121 = CARTESIAN_POINT ( 'NONE',  ( 49.99999999999999289, 37.10000000000000142, -16.24598481164532160 ) ) ;
#16122 = PRESENTATION_STYLE_ASSIGNMENT (( #6149 ) ) ;
#16123 = ORIENTED_EDGE ( 'NONE', *, *, #2785, .F. ) ;
#16124 = CARTESIAN_POINT ( 'NONE',  ( 30.81806926056964002, 30.55937500034139731, 42.41743335407647209 ) ) ;
#16125 = CIRCLE ( 'NONE', #2581, 60.00000000000000711 ) ;
#16126 = EDGE_LOOP ( 'NONE', ( #9131, #3903 ) ) ;
#16127 = VERTEX_POINT ( 'NONE', #15618 ) ;
#16128 = ORIENTED_EDGE ( 'NONE', *, *, #3960, .T. ) ;
#16130 =( BOUNDED_CURVE ( )  B_SPLINE_CURVE ( 3, ( #5675, #15803, #10504, #7918 ),
 .UNSPECIFIED., .F., .T. ) 
 B_SPLINE_CURVE_WITH_KNOTS ( ( 4, 4 ),
 ( 3.141592653589793116, 3.724683441357938829 ),
 .UNSPECIFIED. ) 
 CURVE ( )  GEOMETRIC_REPRESENTATION_ITEM ( )  RATIONAL_B_SPLINE_CURVE ( ( 1.000000000000000000, 0.9718672150731668680, 0.9718672150731668680, 1.000000000000000000 ) ) 
 REPRESENTATION_ITEM ( '' )  );
#16129 = AXIS2_PLACEMENT_3D ( 'NONE', #13682, #10952, #4483 ) ;
#16131 = CARTESIAN_POINT ( 'NONE',  ( -15.45084971874737256, 43.38125000068279746, -47.55282581475767500 ) ) ;
#16132 = CYLINDRICAL_SURFACE ( 'NONE', #7620, 50.00000000000000000 ) ;
#16133 = CARTESIAN_POINT ( 'NONE',  ( 30.90169943749475223, 28.70000000000000284, 42.53254041760199300 ) ) ;
#16134 = ORIENTED_EDGE ( 'NONE', *, *, #14044, .F. ) ;
#16135 = CARTESIAN_POINT ( 'NONE',  ( -15.45084971874737256, 47.38125000068279746, -47.55282581475767500 ) ) ;
#16136 = CARTESIAN_POINT ( 'NONE',  ( -13.33429048796512717, 33.83343271840278277, 101.0000000000000000 ) ) ;
#16137 = DIRECTION ( 'NONE',  ( -0.6691306063588569053, -0.7431448254773954654, 0.000000000000000000 ) ) ;
#16138 = DIRECTION ( 'NONE',  ( 1.000000000000000000, 0.000000000000000000, -0.000000000000000000 ) ) ;
#16139 = DIRECTION ( 'NONE',  ( 0.000000000000000000, 0.000000000000000000, 1.000000000000000000 ) ) ;
#16140 = CARTESIAN_POINT ( 'NONE',  ( 30.90169943749475223, 38.69999999999999574, 42.53254041760199300 ) ) ;
#16141 = DIRECTION ( 'NONE',  ( 0.000000000000000000, 0.000000000000000000, -1.000000000000000000 ) ) ;
#16142 = FACE_OUTER_BOUND ( 'NONE', #4253, .T. ) ;
#16143 = CARTESIAN_POINT ( 'NONE',  ( 9.657523855033129090E-15, 46.28125000068279604, 52.57311121191334990 ) ) ;
#16144 = DIRECTION ( 'NONE',  ( 0.000000000000000000, 0.000000000000000000, 1.000000000000000000 ) ) ;
#16145 = CARTESIAN_POINT ( 'NONE',  ( 50.00000000000000000, 31.00000000000000355, -6.123233995736766085E-15 ) ) ;
#16146 = CARTESIAN_POINT ( 'NONE',  ( 40.34137639590981905, 28.65937500034139873, 29.30972558990010768 ) ) ;
#16147 = DIRECTION ( 'NONE',  ( -0.9510565162951503115, -0.3090169943749574988, 0.000000000000000000 ) ) ;
#16148 = LINE ( 'NONE', #16055, #15737 ) ;
#16149 = VERTEX_POINT ( 'NONE', #4244 ) ;
#16150 = CARTESIAN_POINT ( 'NONE',  ( 40.45084971874737079, 45.20000000000000284, -29.38926261462366440 ) ) ;
#16151 = ORIENTED_EDGE ( 'NONE', *, *, #2274, .T. ) ;
#16152 = DIRECTION ( 'NONE',  ( 0.000000000000000000, 0.000000000000000000, -1.000000000000000000 ) ) ;
#16153 = CARTESIAN_POINT ( 'NONE',  ( 49.86468353125001585, 32.75937500034140015, 16.20201782572375038 ) ) ;
#16154 = CARTESIAN_POINT ( 'NONE',  ( 7.919222016226758143, 40.33250428222964246, 50.00000000000000711 ) ) ;
#16155 = DIRECTION ( 'NONE',  ( 0.9510565162951544194, -0.3090169943749448422, 0.000000000000000000 ) ) ;
#16156 = CARTESIAN_POINT ( 'NONE',  ( 25.00000000000000000, 287.0000000000000000, 7.500000000000000888 ) ) ;
#16157 = DIRECTION ( 'NONE',  ( 0.8660254037844326014, 0.000000000000000000, -0.5000000000000104361 ) ) ;
#16158 = CARTESIAN_POINT ( 'NONE',  ( 15.40903463028481113, 31.32187500034139305, -47.42413220539094709 ) ) ;
#16159 = CARTESIAN_POINT ( 'NONE',  ( 40.34137639590981905, 32.65937500034139873, 29.30972558990010768 ) ) ;
#16160 = CARTESIAN_POINT ( 'NONE',  ( -50.00000000000000000, 36.00000000000000711, 0.000000000000000000 ) ) ;
#16161 = CARTESIAN_POINT ( 'NONE',  ( -49.86468353125000164, 33.92187500034139447, 0.000000000000000000 ) ) ;
#16162 = FACE_OUTER_BOUND ( 'NONE', #1861, .T. ) ;
#16163 = AXIS2_PLACEMENT_3D ( 'NONE', #6163, #8557, #2079 ) ;
#16164 = CARTESIAN_POINT ( 'NONE',  ( 49.86468353124999453, 42.95937500034139589, -16.20201782572376459 ) ) ;
#16165 = CARTESIAN_POINT ( 'NONE',  ( -49.86468353124999453, 38.02187500034140299, 16.20201782572377525 ) ) ;
#16166 = EDGE_CURVE ( 'NONE', #5951, #13593, #12579, .T. ) ;
#16167 = CARTESIAN_POINT ( 'NONE',  ( 30.90169943749475578, 44.69999999999999574, 42.53254041760200010 ) ) ;
#16168 = ORIENTED_EDGE ( 'NONE', *, *, #5698, .T. ) ;
#16169 = CARTESIAN_POINT ( 'NONE',  ( 15.40903463028481113, 45.25937500034140015, -47.42413220539094709 ) ) ;
#16170 = ORIENTED_EDGE ( 'NONE', *, *, #10694, .F. ) ;
#16172 = ADVANCED_FACE ( 'NONE', ( #7221 ), #13363, .F. ) ;
#16171 = CARTESIAN_POINT ( 'NONE',  ( 15.45084971874737789, 26.38125000068280102, 47.55282581475767500 ) ) ;
#16173 = EDGE_CURVE ( 'NONE', #895, #1641, #12204, .T. ) ;
#16174 = ORIENTED_EDGE ( 'NONE', *, *, #1271, .T. ) ;
#16175 = DIRECTION ( 'NONE',  ( -0.000000000000000000, 1.000000000000000000, -0.000000000000000000 ) ) ;
#16176 = CARTESIAN_POINT ( 'NONE',  ( -40.34137639590981905, 33.72187500034139873, -29.30972558990011478 ) ) ;
#16177 = EDGE_CURVE ( 'NONE', #15517, #4175, #12281, .T. ) ;
#16178 = CARTESIAN_POINT ( 'NONE',  ( 49.86468353125001585, 48.82187500034139305, 16.20201782572375038 ) ) ;
#16179 = CARTESIAN_POINT ( 'NONE',  ( 7.919222016226940219, 31.44874571845315714, -49.99999999999996447 ) ) ;
#16180 = CARTESIAN_POINT ( 'NONE',  ( -15.40903463028481646, 25.52187500034139589, -47.42413220539093999 ) ) ;
#16181 = CARTESIAN_POINT ( 'NONE',  ( 50.00000000000000000, 32.78125000068279604, -6.123233995736766085E-15 ) ) ;
#16182 = AXIS2_PLACEMENT_3D ( 'NONE', #2384, #7710, #12615 ) ;
#16183 = CARTESIAN_POINT ( 'NONE',  ( 15.40903463028482356, 40.52187500034139589, 47.42413220539093999 ) ) ;
#16184 = FACE_OUTER_BOUND ( 'NONE', #13292, .T. ) ;
#16185 = ORIENTED_EDGE ( 'NONE', *, *, #12934, .F. ) ;
#16186 = CARTESIAN_POINT ( 'NONE',  ( -3.210462471511496205E-15, 37.42187500034140157, -52.43083105670540789 ) ) ;
#16187 = CARTESIAN_POINT ( 'NONE',  ( 24.14213562373095101, 282.0000000000000000, -9.571067811865473729 ) ) ;
#16188 = VERTEX_POINT ( 'NONE', #14767 ) ;
#16189 = ORIENTED_EDGE ( 'NONE', *, *, #1424, .T. ) ;
#16190 = ORIENTED_EDGE ( 'NONE', *, *, #12818, .T. ) ;
#16191 = LINE ( 'NONE', #801, #5775 ) ;
#16192 = CARTESIAN_POINT ( 'NONE',  ( -8.660254037844387298, 25.00000000000000355, 5.000000000000000000 ) ) ;
#16193 = CARTESIAN_POINT ( 'NONE',  ( 50.00000000000000000, 27.00000000000000355, -6.123233995736766085E-15 ) ) ;
#16194 = DIRECTION ( 'NONE',  ( 0.000000000000000000, 0.000000000000000000, 1.000000000000000000 ) ) ;
#16195 = AXIS2_PLACEMENT_3D ( 'NONE', #8214, #5493, #11876 ) ;
#16196 = CARTESIAN_POINT ( 'NONE',  ( 30.81806926056964002, 38.55937500034140442, 42.41743335407647209 ) ) ;
#16197 = CARTESIAN_POINT ( 'NONE',  ( -15.40903463028481646, 43.45937500034139589, -47.42413220539093999 ) ) ;
#16198 = CARTESIAN_POINT ( 'NONE',  ( -7.500000000000005329, 25.00000000000000355, 24.29058411375428506 ) ) ;
#16199 = CARTESIAN_POINT ( 'NONE',  ( -30.90169943749473447, 40.30000000000000426, 42.53254041760200721 ) ) ;
#16200 = CARTESIAN_POINT ( 'NONE',  ( 49.99999999999999289, 41.10000000000000142, -16.24598481164532160 ) ) ;
#16201 = DIRECTION ( 'NONE',  ( 0.000000000000000000, -0.6143407043256605693, 0.7890408728378088821 ) ) ;
#16202 = VERTEX_POINT ( 'NONE', #5811 ) ;
#16203 = CARTESIAN_POINT ( 'NONE',  ( -3.210462471511496205E-15, 25.35937500034139802, -52.43083105670540789 ) ) ;
#16204 = EDGE_LOOP ( 'NONE', ( #900, #11805, #2685, #11208 ) ) ;
#16205 = ORIENTED_EDGE ( 'NONE', *, *, #15012, .F. ) ;
#16206 = ORIENTED_EDGE ( 'NONE', *, *, #1806, .F. ) ;
#16207 = CARTESIAN_POINT ( 'NONE',  ( 50.00000000000000000, 46.78125000068279604, -6.123233995736766085E-15 ) ) ;
#16208 = PLANE ( 'NONE',  #12409 ) ;
#16209 = DIRECTION ( 'NONE',  ( 0.000000000000000000, 0.000000000000000000, 1.000000000000000000 ) ) ;
#16210 = ORIENTED_EDGE ( 'NONE', *, *, #8343, .T. ) ;
#16211 = CARTESIAN_POINT ( 'NONE',  ( -30.90169943749473447, 28.08125000068280031, 42.53254041760200721 ) ) ;
#16212 = DIRECTION ( 'NONE',  ( 0.9781476007338070211, -0.2079116908177531808, -0.000000000000000000 ) ) ;
#16213 = LINE ( 'NONE', #2154, #7063 ) ;
#16214 = CARTESIAN_POINT ( 'NONE',  ( 0.000000000000000000, 274.0000000000000000, 0.000000000000000000 ) ) ;
#16215 = CARTESIAN_POINT ( 'NONE',  ( 7.394441145214595501, 28.48516834767053751, 101.0000000000000000 ) ) ;
#16216 = PLANE ( 'NONE',  #4174 ) ;
#16217 = EDGE_CURVE ( 'NONE', #4275, #6384, #6978, .T. ) ;
#16218 = CARTESIAN_POINT ( 'NONE',  ( 40.45084971874737789, 46.80000000000000426, 29.38926261462365375 ) ) ;
#16219 = CARTESIAN_POINT ( 'NONE',  ( 15.45084971874737789, 44.38125000068279746, 47.55282581475767500 ) ) ;
#16220 = FACE_OUTER_BOUND ( 'NONE', #9996, .T. ) ;
#16221 = CARTESIAN_POINT ( 'NONE',  ( 50.00000000000000711, 30.89999999999999503, 16.24598481164530739 ) ) ;
#16222 = CARTESIAN_POINT ( 'NONE',  ( 15.40903463028482356, 20.45937500034139589, 47.42413220539093999 ) ) ;
#16223 = CARTESIAN_POINT ( 'NONE',  ( 0.000000000000000000, 22.50000000000000000, 100.0000000000000000 ) ) ;
#16224 =( BOUNDED_CURVE ( )  B_SPLINE_CURVE ( 2, ( #803, #2381, #11040, #13444, #9712, #6141, #2298, #6063, #7464, #12531, #5891, #14763, #12200 ),
 .UNSPECIFIED., .F., .T. ) 
 B_SPLINE_CURVE_WITH_KNOTS ( ( 3, 2, 2, 2, 2, 2, 3 ),
 ( 0.9166666666666667407, 0.9200000000000000400, 0.9266666666666666385, 0.9333333333333333481, 0.9399999999999999467, 0.9466666666666666563, 0.9500000000000000666 ),
 .UNSPECIFIED. ) 
 CURVE ( )  GEOMETRIC_REPRESENTATION_ITEM ( )  RATIONAL_B_SPLINE_CURVE ( ( 0.9755282581475768211, 0.9755282581475771542, 1.000000000000000000, 0.9510565162951535312, 1.000000000000000000, 0.9510565162951535312, 1.000000000000000000, 0.9510565162951535312, 1.000000000000000000, 0.9510565162951535312, 1.000000000000000000, 0.9755282581475763770, 0.9755282581475768211 ) ) 
 REPRESENTATION_ITEM ( '' )  );
#16225 = CARTESIAN_POINT ( 'NONE',  ( 15.40903463028482356, 42.45937500034140299, 47.42413220539093999 ) ) ;
#16226 = VERTEX_POINT ( 'NONE', #15866 ) ;
#16227 = DIRECTION ( 'NONE',  ( -6.938893903907231459E-18, 1.000000000000000000, 5.551115123125782702E-17 ) ) ;
#16228 = EDGE_LOOP ( 'NONE', ( #10101, #6154, #6867, #4171 ) ) ;
#16229 = CARTESIAN_POINT ( 'NONE',  ( 15.45084971874737789, 48.60000000000000142, 47.55282581475767500 ) ) ;
#16230 = CARTESIAN_POINT ( 'NONE',  ( 15.40903463028482356, 36.45937500034139589, 47.42413220539093999 ) ) ;
#16231 = CARTESIAN_POINT ( 'NONE',  ( 0.000000000000000000, 22.50000000000000000, 102.0000000000000142 ) ) ;
#16232 = PLANE ( 'NONE',  #11837 ) ;
#16233 = CARTESIAN_POINT ( 'NONE',  ( -3.111920190527341144E-15, 29.28125000068279604, -50.00000000000000000 ) ) ;
#16234 = CARTESIAN_POINT ( 'NONE',  ( 30.90169943749475223, 44.48125000068279888, 42.53254041760199300 ) ) ;
#16235 = CARTESIAN_POINT ( 'NONE',  ( 30.81806926056964002, 20.62187500034139020, 42.41743335407647209 ) ) ;
#16236 = CARTESIAN_POINT ( 'NONE',  ( -3.210462471511496205E-15, 31.35937500034138736, -52.43083105670540789 ) ) ;
#16237 = CARTESIAN_POINT ( 'NONE',  ( 7.580410092413998768, 99.32916037694960210, -5.000000000000000000 ) ) ;
#16238 = CARTESIAN_POINT ( 'NONE',  ( -15.40903463028481646, 35.52187500034139589, -47.42413220539093999 ) ) ;
#16239 = CARTESIAN_POINT ( 'NONE',  ( -8.487905985326110070, 94.05711243240941144, -4.885539557155581747 ) ) ;
#16240 = CARTESIAN_POINT ( 'NONE',  ( 15.40903463028481113, 41.25937500034139305, -47.42413220539094709 ) ) ;
#16241 = CARTESIAN_POINT ( 'NONE',  ( -40.34137639590981905, 39.72187500034139873, -29.30972558990011478 ) ) ;
#16242 = CARTESIAN_POINT ( 'NONE',  ( -30.90169943749474868, 43.70000000000000284, -42.53254041760200721 ) ) ;
#16243 = EDGE_LOOP ( 'NONE', ( #2317, #12066, #7721, #4061 ) ) ;
#16244 = EDGE_CURVE ( 'NONE', #12025, #15727, #4480, .T. ) ;
#16245 = CARTESIAN_POINT ( 'NONE',  ( -49.86468353124999453, 41.75937500034139305, -16.20201782572375393 ) ) ;
#16246 = VERTEX_POINT ( 'NONE', #10500 ) ;
#16247 = CARTESIAN_POINT ( 'NONE',  ( -3.219174618344376363E-15, 25.28125000068279604, -52.57311121191334990 ) ) ;
#16248 = CARTESIAN_POINT ( 'NONE',  ( -7.919222016226934890, 34.44874571845316069, 49.99999999999996447 ) ) ;
#16249 = CARTESIAN_POINT ( 'NONE',  ( 49.99999999999999289, 40.88125000068279746, -16.24598481164532160 ) ) ;
#16250 = CARTESIAN_POINT ( 'NONE',  ( -49.86468353124999453, 42.02187500034139589, 16.20201782572377525 ) ) ;
#16251 = CARTESIAN_POINT ( 'NONE',  ( 7.580410092413998768, 101.3368000520362813, -5.000000000000000000 ) ) ;
#16252 = CARTESIAN_POINT ( 'NONE',  ( -40.34137639590981195, 26.12187500034139731, 29.30972558990012189 ) ) ;
#16253 = CARTESIAN_POINT ( 'NONE',  ( -49.99999999999999289, 27.68125000068279462, -16.24598481164531449 ) ) ;
#16254 = ADVANCED_FACE ( 'NONE', ( #4347 ), #15643, .T. ) ;
#16255 = CARTESIAN_POINT ( 'NONE',  ( -40.34137639590981905, 33.72187500034139873, -29.30972558990011478 ) ) ;
#16256 = CARTESIAN_POINT ( 'NONE',  ( -21.01167039530930936, 284.7842439685843487, -8.005835197660415403 ) ) ;
#16257 = CARTESIAN_POINT ( 'NONE',  ( 40.34137639590981195, 35.12187500034139731, -29.30972558990011834 ) ) ;
#16258 = CARTESIAN_POINT ( 'NONE',  ( -50.00000000000000000, 31.78125000068279959, 0.000000000000000000 ) ) ;
#16259 = EDGE_CURVE ( 'NONE', #13440, #3318, #11188, .T. ) ;
#16260 = ORIENTED_EDGE ( 'NONE', *, *, #15184, .F. ) ;
#16261 = ORIENTED_EDGE ( 'NONE', *, *, #15446, .F. ) ;
#16262 =( BOUNDED_CURVE ( )  B_SPLINE_CURVE ( 2, ( #10565, #4321, #3991, #13046, #10471, #11714, #1648, #2731, #8050, #6745, #15449, #11640, #14363 ),
 .UNSPECIFIED., .F., .F. ) 
 B_SPLINE_CURVE_WITH_KNOTS ( ( 3, 2, 2, 2, 2, 2, 3 ),
 ( 0.7833333333333333259, 0.7866666666666666252, 0.7933333333333333348, 0.8000000000000000444, 0.8066666666666666430, 0.8133333333333333526, 0.8166666666666666519 ),
 .UNSPECIFIED. ) 
 CURVE ( )  GEOMETRIC_REPRESENTATION_ITEM ( )  RATIONAL_B_SPLINE_CURVE ( ( 0.9755282581475768211, 0.9755282581475768211, 1.000000000000000000, 0.9510565162951535312, 1.000000000000000000, 0.9510565162951535312, 1.000000000000000000, 0.9510565162951535312, 1.000000000000000000, 0.9510565162951535312, 1.000000000000000000, 0.9755282581475768211, 0.9755282581475768211 ) ) 
 REPRESENTATION_ITEM ( '' )  );
#16263 = CIRCLE ( 'NONE', #9365, 85.01963570546854498 ) ;
#16264 = VERTEX_POINT ( 'NONE', #14309 ) ;
#16265 = CARTESIAN_POINT ( 'NONE',  ( -40.45084971874737789, 31.80000000000000071, -29.38926261462365730 ) ) ;
#16266 = CYLINDRICAL_SURFACE ( 'NONE', #121, 2.000000000000001776 ) ;
#16267 = EDGE_CURVE ( 'NONE', #8227, #12043, #10188, .T. ) ;
#16268 = PLANE ( 'NONE',  #6548 ) ;
#16269 = DIRECTION ( 'NONE',  ( 0.000000000000000000, 0.000000000000000000, 1.000000000000000000 ) ) ;
#16270 = CARTESIAN_POINT ( 'NONE',  ( -40.34137639590981195, 36.05937500034139731, 29.30972558990012189 ) ) ;
#16271 = CARTESIAN_POINT ( 'NONE',  ( 49.86468353125001585, 40.75937500034138594, 16.20201782572375038 ) ) ;
#16272 = PRESENTATION_STYLE_ASSIGNMENT (( #1051 ) ) ;
#16273 = CARTESIAN_POINT ( 'NONE',  ( 0.000000000000000000, 0.000000000000000000, 0.000000000000000000 ) ) ;
#16274 = CARTESIAN_POINT ( 'NONE',  ( 0.000000000000000000, 25.00000000000000000, 0.000000000000000000 ) ) ;
#16275 = VECTOR ( 'NONE', #4090, 1000.000000000000000 ) ;
#16276 = CARTESIAN_POINT ( 'NONE',  ( 9.881733417930924190, 8.048309972292271297, 101.0000000000000000 ) ) ;
#16277 = ORIENTED_EDGE ( 'NONE', *, *, #12839, .F. ) ;
#16278 = EDGE_CURVE ( 'NONE', #13988, #9739, #5362, .T. ) ;
#16279 = CARTESIAN_POINT ( 'NONE',  ( 49.86468353125001585, 24.75937500034140015, 16.20201782572375038 ) ) ;
#16280 = EDGE_LOOP ( 'NONE', ( #13597, #4661, #11477, #3572 ) ) ;
#16281 = VERTEX_POINT ( 'NONE', #5600 ) ;
#16282 = ORIENTED_EDGE ( 'NONE', *, *, #2912, .F. ) ;
#16283 = CARTESIAN_POINT ( 'NONE',  ( -40.45084971874737079, 37.98125000068279888, 29.38926261462367151 ) ) ;
#16284 = CARTESIAN_POINT ( 'NONE',  ( -24.78626291527393022, 40.00000000000000711, -5.650101528493793879 ) ) ;
#16285 = CARTESIAN_POINT ( 'NONE',  ( 7.436122194756328518, 37.97250723688144802, 101.3333374614808662 ) ) ;
#16286 = EDGE_CURVE ( 'NONE', #12958, #7234, #10665, .T. ) ;
#16288 = ORIENTED_EDGE ( 'NONE', *, *, #3765, .F. ) ;
#16287 = TOROIDAL_SURFACE ( 'NONE', #1410, 87.81953344283027718, 2.000000000000000000 ) ;
#16289 = CARTESIAN_POINT ( 'NONE',  ( 0.000000000000000000, 20.00000000000000355, 50.00000000000000000 ) ) ;
#16290 = CARTESIAN_POINT ( 'NONE',  ( 0.000000000000000000, 20.00000000000000355, 50.00000000000000000 ) ) ;
#16291 = CARTESIAN_POINT ( 'NONE',  ( -20.00000000000000355, 312.0000000000000568, 2.500000000000001332 ) ) ;
#16292 = CARTESIAN_POINT ( 'NONE',  ( 2.600676159226421000E-13, 23.28125000068279604, -49.99999999999999289 ) ) ;
#16293 = CARTESIAN_POINT ( 'NONE',  ( 20.00000000000000000, 307.0000000000000568, 2.500000000000002220 ) ) ;
#16294 = CARTESIAN_POINT ( 'NONE',  ( -3.111920190527341144E-15, 25.28125000068279604, -50.00000000000000000 ) ) ;
#16295 = DIRECTION ( 'NONE',  ( -0.000000000000000000, 1.000000000000000000, 0.000000000000000000 ) ) ;
#16296 = CYLINDRICAL_SURFACE ( 'NONE', #2760, 40.00000000000000000 ) ;
#16297 = CARTESIAN_POINT ( 'NONE',  ( 30.90169943749474157, 49.08125000068280031, -42.53254041760200721 ) ) ;
#16298 = CARTESIAN_POINT ( 'NONE',  ( 40.45084971874737789, 20.80000000000000426, 29.38926261462365375 ) ) ;
#16299 = CARTESIAN_POINT ( 'NONE',  ( 15.45084971874736723, 29.40000000000000213, -47.55282581475768211 ) ) ;
#16300 = CARTESIAN_POINT ( 'NONE',  ( 15.40903463028482356, 22.45937500034139589, 47.42413220539093999 ) ) ;
#16301 = EDGE_CURVE ( 'NONE', #7423, #10059, #12297, .T. ) ;
#16302 = DIRECTION ( 'NONE',  ( -0.7431448254773861395, -0.6691306063588672304, 0.000000000000000000 ) ) ;
#16303 = AXIS2_PLACEMENT_3D ( 'NONE', #15779, #10960, #8541 ) ;
#16304 = CARTESIAN_POINT ( 'NONE',  ( 15.40903463028482356, 46.45937500034139589, 47.42413220539093999 ) ) ;
#16305 = EDGE_LOOP ( 'NONE', ( #6780, #5311 ) ) ;
#16306 = CARTESIAN_POINT ( 'NONE',  ( 7.919222016226854954, 42.33250428222964246, 49.99999999999998579 ) ) ;
#16307 = ORIENTED_EDGE ( 'NONE', *, *, #5316, .T. ) ;
#16308 =( REPRESENTATION_RELATIONSHIP ('NONE','NONE', #6178, #15095 ) REPRESENTATION_RELATIONSHIP_WITH_TRANSFORMATION ( #2195 )SHAPE_REPRESENTATION_RELATIONSHIP( ) );
#16309 = DIRECTION ( 'NONE',  ( 0.000000000000000000, 0.000000000000000000, 1.000000000000000000 ) ) ;
#16310 = CARTESIAN_POINT ( 'NONE',  ( 15.40903463028481113, 37.25937500034140015, -47.42413220539094709 ) ) ;
#16311 = CARTESIAN_POINT ( 'NONE',  ( 8.880528407616436581, 25.91118970470966687, 102.0000000000000142 ) ) ;
#16312 = DIRECTION ( 'NONE',  ( -0.000000000000000000, 1.000000000000000000, -0.000000000000000000 ) ) ;
#16313 = CARTESIAN_POINT ( 'NONE',  ( 46.19495089481205241, 24.99999999999999289, -18.77607397657055799 ) ) ;
#16314 = AXIS2_PLACEMENT_3D ( 'NONE', #7607, #9021, #13751 ) ;
#16315 = CARTESIAN_POINT ( 'NONE',  ( 30.90169943749473802, 47.08125000068280031, -42.53254041760200721 ) ) ;
#16316 = CARTESIAN_POINT ( 'NONE',  ( -30.81806926056963292, 23.62187500034139731, -42.41743335407647209 ) ) ;
#16317 = CARTESIAN_POINT ( 'NONE',  ( 15.40903463028481113, 29.25937500034139660, -47.42413220539094709 ) ) ;
#16318 = DIRECTION ( 'NONE',  ( 0.3535533905932762289, 0.7071067811865484609, 0.6123724356957919168 ) ) ;
#16319 = CARTESIAN_POINT ( 'NONE',  ( 49.86468353124999453, 35.02187500034139589, -16.20201782572376104 ) ) ;
#16320 = CARTESIAN_POINT ( 'NONE',  ( -30.90169943749473447, 30.08125000068279675, 42.53254041760200721 ) ) ;
#16321 = CARTESIAN_POINT ( 'NONE',  ( -30.90169943749474868, 37.70000000000000995, -42.53254041760200721 ) ) ;
#16322 = CARTESIAN_POINT ( 'NONE',  ( -49.86468353125000164, 37.85937500034139447, 0.000000000000000000 ) ) ;
#16323 = CARTESIAN_POINT ( 'NONE',  ( 15.40903463028481113, 37.32187500034140015, -47.42413220539094709 ) ) ;
#16324 = CARTESIAN_POINT ( 'NONE',  ( 15.45084971874737789, 46.60000000000000142, 47.55282581475767500 ) ) ;
#16325 = ORIENTED_EDGE ( 'NONE', *, *, #16374, .F. ) ;
#16326 = AXIS2_PLACEMENT_3D ( 'NONE', #3496, #8633, #7237 ) ;
#16327 = CARTESIAN_POINT ( 'NONE',  ( 40.34137639590981905, 40.65937500034139873, 29.30972558990010768 ) ) ;
#16328 = EDGE_LOOP ( 'NONE', ( #5143, #7300, #8456, #5026 ) ) ;
#16329 = CARTESIAN_POINT ( 'NONE',  ( -40.45084971874737079, 25.98125000068279888, 29.38926261462367151 ) ) ;
#16330 = CARTESIAN_POINT ( 'NONE',  ( -49.99999999999999289, 34.10000000000000853, 16.24598481164533226 ) ) ;
#16331 = CARTESIAN_POINT ( 'NONE',  ( 40.34137639590981905, 22.72187500034139518, 29.30972558990010768 ) ) ;
#16332 = DIRECTION ( 'NONE',  ( 0.000000000000000000, 0.000000000000000000, -1.000000000000000000 ) ) ;
#16333 = CARTESIAN_POINT ( 'NONE',  ( 40.34137639590981195, 41.12187500034139731, -29.30972558990011834 ) ) ;
#16334 = CARTESIAN_POINT ( 'NONE',  ( 9.735664389687646693E-15, 262.0000000000000000, -79.49773270518484480 ) ) ;
#16335 = VECTOR ( 'NONE', #12609, 999.9999999999998863 ) ;
#16336 = CARTESIAN_POINT ( 'NONE',  ( 9.631387414534489405E-15, 20.42187500034139802, 52.43083105670540789 ) ) ;
#16337 = CARTESIAN_POINT ( 'NONE',  ( 40.45084971874737789, 24.58125000068280031, 29.38926261462365375 ) ) ;
#16338 = CARTESIAN_POINT ( 'NONE',  ( -3.210462471511496205E-15, 35.42187500034140157, -52.43083105670540789 ) ) ;
#16339 = DIRECTION ( 'NONE',  ( -0.000000000000000000, -1.000000000000000000, -0.000000000000000000 ) ) ;
#16340 = CARTESIAN_POINT ( 'NONE',  ( -49.86468353124999453, 33.82187500034138594, -16.20201782572375393 ) ) ;
#16341 = CARTESIAN_POINT ( 'NONE',  ( -40.45084971874737079, 41.98125000068279888, 29.38926261462367151 ) ) ;
#16342 = ORIENTED_EDGE ( 'NONE', *, *, #7778, .F. ) ;
#16343 = CONICAL_SURFACE ( 'NONE', #9186, 65.00000000000000000, 0.08726646259971666819 ) ;
#16344 = ORIENTED_EDGE ( 'NONE', *, *, #8539, .T. ) ;
#16345 = ADVANCED_FACE ( 'NONE', ( #10417 ), #9165, .F. ) ;
#16346 = PRODUCT_DEFINITION_FORMATION_WITH_SPECIFIED_SOURCE ( 'ANY', '', #6681, .NOT_KNOWN. ) ;
#16347 = CARTESIAN_POINT ( 'NONE',  ( 0.000000000000000000, 262.0000000000000000, 0.000000000000000000 ) ) ;
#16348 = DIRECTION ( 'NONE',  ( -3.536495997885206014E-17, -0.9396926207859082059, -0.3420201433256695456 ) ) ;
#16349 = CARTESIAN_POINT ( 'NONE',  ( 9.395693774364776374, 21.00971865127324634, 101.0000000000000000 ) ) ;
#16350 = DIRECTION ( 'NONE',  ( 0.000000000000000000, 1.000000000000000000, 0.000000000000000000 ) ) ;
#16351 = VECTOR ( 'NONE', #5457, 1000.000000000000227 ) ;
#16352 = CARTESIAN_POINT ( 'NONE',  ( 30.81806926056962936, 33.15937500034139873, -42.41743335407647209 ) ) ;
#16353 = CARTESIAN_POINT ( 'NONE',  ( -25.00000000000000355, 307.0000000000000568, -7.499999999999999112 ) ) ;
#16354 = CARTESIAN_POINT ( 'NONE',  ( 30.81806926056964002, 48.62187500034139731, 42.41743335407646498 ) ) ;
#16355 = DIRECTION ( 'NONE',  ( 0.000000000000000000, 0.000000000000000000, 1.000000000000000000 ) ) ;
#16356 = VECTOR ( 'NONE', #3827, 1000.000000000000000 ) ;
#16357 = FACE_OUTER_BOUND ( 'NONE', #15786, .T. ) ;
#16358 = CARTESIAN_POINT ( 'NONE',  ( -40.45084971874737789, 41.80000000000000426, -29.38926261462365730 ) ) ;
#16359 = ORIENTED_EDGE ( 'NONE', *, *, #15755, .F. ) ;
#16360 =( BOUNDED_CURVE ( )  B_SPLINE_CURVE ( 2, ( #13608, #973, #4747, #6069, #9882, #10296, #1381, #3970, #12780, #6563, #7711, #11293, #15261, #16354, #6224, #10210, #9120, #11529, #12862, #4994, #5152, #219, #12701, #2465, #15351, #3890, #15179, #1467, #5076, #1128, #10129, #48, #6391, #1215, #10049, #11453, #3729, #6472, #11621, #7547, #2551, #8962, #8789, #7872, #5322, #14018, #3809, #10374, #9043, #14181, #14098, #128, #2712, #15103, #15431, #2634, #13852, #8874, #4051, #12616, #7791, #5241, #7634, #2798, #6312, #11378, #16442, #1300, #13932, #2888, #7956, #15510, #14266, #11772, #13029, #11696, #9211, #11940, #4138, #4225, #1630, #463, #3043, #4306, #5565, #6648, #2966, #10626, #9371, #15679, #14420, #6726, #8113, #8032, #297, #374, #13192, #5394, #13107, #10546, #5476, #1797, #6889, #541, #15604, #12951, #9293, #14348, #1554, #10453, #1712, #6808, #11860, #7360, #11421, #13817, #2510, #10171, #4954, #12667, #4872, #14, #12746, #5116, #2429, #3527, #15221, #8673, #2599, #13981, #1265, #6113, #2262, #11183, #4792, #2353, #10014, #3851, #12502, #7435, #1016, #9848, #6356, #7675, #16238, #6270, #7506, #12577, #6187, #16319, #8579, #3772, #11342, #13894, #16409, #8916, #1175, #14900, #8754, #13654, #16161, #1343, #5041, #11101, #12425, #15069, #3698, #1095, #11261, #9928, #7589, #10095, #14982, #3611, #8831, #15144, #13740, #424, #9167, #2758, #15397, #9006, #12992, #1675, #7753, #7833, #15313, #1423, #13072, #3934, #4095, #14063, #14142, #7917, #12908, #2679, #6516, #6774, #12822, #14223, #11574, #10589, #4190, #14386, #14311, #1596, #2931, #10250, #5528, #11662, #181, #4017, #15645, #5285, #15561, #4270, #11818, #9256, #10336, #2849, #7998, #1518, #6608, #9086, #13151, #6690, #259, #91, #15474, #5195, #3007, #5364, #10420, #11738, #9335, #8077, #6434, #341, #11493, #5439, #10502, #10906, #7171, #13476, #12232, #3091, #14460, #2082, #4516, #9655, #835, #12060, #3336, #11983, #11907, #13387, #4432, #9413, #13311, #7004, #6859, #9749, #4678, #8407, #13237, #8168, #1835, #505, #9502, #663, #5925, #3175, #14548, #6931, #14794, #1910, #10667, #8322, #580, #5602, #5760, #10829, #15893, #15718, #15969, #1995, #4590, #7091, #10985, #12151, #4349, #9581, #5674, #10743, #14626, #3428, #753, #16049, #15802, #3252, #5841 ),
 .UNSPECIFIED., .F., .F. ) 
 B_SPLINE_CURVE_WITH_KNOTS ( ( 3, 2, 2, 2, 2, 2, 2, 2, 2, 2, 2, 2, 2, 2, 2, 2, 2, 2, 2, 2, 2, 2, 2, 2, 2, 2, 2, 2, 2, 2, 2, 2, 2, 2, 2, 2, 2, 2, 2, 2, 2, 2, 2, 2, 2, 2, 2, 2, 2, 2, 2, 2, 2, 2, 2, 2, 2, 2, 2, 2, 2, 2, 2, 2, 2, 2, 2, 2, 2, 2, 2, 2, 2, 2, 2, 2, 2, 2, 2, 2, 2, 2, 2, 2, 2, 2, 2, 2, 2, 2, 2, 2, 2, 2, 2, 2, 2, 2, 2, 2, 2, 2, 2, 2, 2, 2, 2, 2, 2, 2, 2, 2, 2, 2, 2, 2, 2, 2, 2, 2, 2, 2, 2, 2, 2, 2, 2, 2, 2, 2, 2, 2, 2, 2, 2, 2, 2, 2, 2, 2, 2, 2, 2, 2, 2, 2, 2, 2, 2, 2, 3 ),
 ( 0.000000000000000000, 0.006666666666666667095, 0.01333333333333333419, 0.02000000000000000042, 0.02666666666666666838, 0.03333333333333333287, 0.04000000000000000083, 0.04666666666666666879, 0.05333333333333333676, 0.05999999999999999778, 0.06666666666666666574, 0.07333333333333333370, 0.08000000000000000167, 0.08666666666666666963, 0.09333333333333333759, 0.1000000000000000056, 0.1066666666666666735, 0.1133333333333333276, 0.1199999999999999956, 0.1266666666666666774, 0.1333333333333333315, 0.1400000000000000133, 0.1466666666666666674, 0.1533333333333333215, 0.1600000000000000033, 0.1666666666666666574, 0.1733333333333333393, 0.1799999999999999933, 0.1866666666666666752, 0.1933333333333333293, 0.2000000000000000111, 0.2066666666666666652, 0.2133333333333333470, 0.2200000000000000011, 0.2266666666666666552, 0.2333333333333333370, 0.2399999999999999911, 0.2466666666666666730, 0.2533333333333333548, 0.2600000000000000089, 0.2666666666666666630, 0.2733333333333333171, 0.2800000000000000266, 0.2866666666666666807, 0.2933333333333333348, 0.2999999999999999889, 0.3066666666666666430, 0.3133333333333333526, 0.3200000000000000067, 0.3266666666666666607, 0.3333333333333333148, 0.3400000000000000244, 0.3466666666666666785, 0.3533333333333333326, 0.3599999999999999867, 0.3666666666666666408, 0.3733333333333333504, 0.3800000000000000044, 0.3866666666666666585, 0.3933333333333333126, 0.4000000000000000222, 0.4066666666666666763, 0.4133333333333333304, 0.4199999999999999845, 0.4266666666666666941, 0.4333333333333333481, 0.4400000000000000022, 0.4466666666666666563, 0.4533333333333333104, 0.4600000000000000200, 0.4666666666666666741, 0.4733333333333333282, 0.4799999999999999822, 0.4866666666666666918, 0.4933333333333333459, 0.5000000000000000000, 0.5066666666666667096, 0.5133333333333333082, 0.5200000000000000178, 0.5266666666666666163, 0.5333333333333333259, 0.5400000000000000355, 0.5466666666666666341, 0.5533333333333333437, 0.5600000000000000533, 0.5666666666666666519, 0.5733333333333333615, 0.5799999999999999600, 0.5866666666666666696, 0.5933333333333333792, 0.5999999999999999778, 0.6066666666666666874, 0.6133333333333332860, 0.6199999999999999956, 0.6266666666666667052, 0.6333333333333333037, 0.6400000000000000133, 0.6466666666666666119, 0.6533333333333333215, 0.6600000000000000311, 0.6666666666666666297, 0.6733333333333333393, 0.6800000000000000488, 0.6866666666666666474, 0.6933333333333333570, 0.6999999999999999556, 0.7066666666666666652, 0.7133333333333333748, 0.7199999999999999734, 0.7266666666666666829, 0.7333333333333332815, 0.7399999999999999911, 0.7466666666666667007, 0.7533333333333332993, 0.7600000000000000089, 0.7666666666666667185, 0.7733333333333333171, 0.7800000000000000266, 0.7866666666666666252, 0.7933333333333333348, 0.8000000000000000444, 0.8066666666666666430, 0.8133333333333333526, 0.8199999999999999512, 0.8266666666666666607, 0.8333333333333333703, 0.8399999999999999689, 0.8466666666666666785, 0.8533333333333333881, 0.8599999999999999867, 0.8666666666666666963, 0.8733333333333332948, 0.8800000000000000044, 0.8866666666666667140, 0.8933333333333333126, 0.9000000000000000222, 0.9066666666666666208, 0.9133333333333333304, 0.9200000000000000400, 0.9266666666666666385, 0.9333333333333333481, 0.9399999999999999467, 0.9466666666666666563, 0.9533333333333333659, 0.9599999999999999645, 0.9666666666666666741, 0.9733333333333333837, 0.9799999999999999822, 0.9866666666666666918, 0.9933333333333332904, 0.9973788038104776099 ),
 .UNSPECIFIED. ) 
 CURVE ( )  GEOMETRIC_REPRESENTATION_ITEM ( )  RATIONAL_B_SPLINE_CURVE ( ( 1.000000000000000000, 0.9510565162951535312, 1.000000000000000000, 0.9510565162951535312, 1.000000000000000000, 0.9510565162951535312, 1.000000000000000000, 0.9510565162951535312, 1.000000000000000000, 0.9510565162951535312, 1.000000000000000000, 0.9510565162951535312, 1.000000000000000000, 0.9510565162951535312, 1.000000000000000000, 0.9510565162951535312, 1.000000000000000000, 0.9510565162951535312, 1.000000000000000000, 0.9510565162951535312, 1.000000000000000000, 0.9510565162951535312, 1.000000000000000000, 0.9510565162951535312, 1.000000000000000000, 0.9510565162951535312, 1.000000000000000000, 0.9510565162951535312, 1.000000000000000000, 0.9510565162951535312, 1.000000000000000000, 0.9510565162951535312, 1.000000000000000000, 0.9510565162951535312, 1.000000000000000000, 0.9510565162951535312, 1.000000000000000000, 0.9510565162951535312, 1.000000000000000000, 0.9510565162951535312, 1.000000000000000000, 0.9510565162951535312, 1.000000000000000000, 0.9510565162951535312, 1.000000000000000000, 0.9510565162951535312, 1.000000000000000000, 0.9510565162951535312, 1.000000000000000000, 0.9510565162951535312, 1.000000000000000000, 0.9510565162951535312, 1.000000000000000000, 0.9510565162951535312, 1.000000000000000000, 0.9510565162951535312, 1.000000000000000000, 0.9510565162951535312, 1.000000000000000000, 0.9510565162951535312, 1.000000000000000000, 0.9510565162951535312, 1.000000000000000000, 0.9510565162951535312, 1.000000000000000000, 0.9510565162951535312, 1.000000000000000000, 0.9510565162951535312, 1.000000000000000000, 0.9510565162951535312, 1.000000000000000000, 0.9510565162951535312, 1.000000000000000000, 0.9510565162951535312, 1.000000000000000000, 0.9510565162951535312, 1.000000000000000000, 0.9510565162951535312, 1.000000000000000000, 0.9510565162951535312, 1.000000000000000000, 0.9510565162951535312, 1.000000000000000000, 0.9510565162951535312, 1.000000000000000000, 0.9510565162951535312, 1.000000000000000000, 0.9510565162951535312, 1.000000000000000000, 0.9510565162951535312, 1.000000000000000000, 0.9510565162951535312, 1.000000000000000000, 0.9510565162951535312, 1.000000000000000000, 0.9510565162951535312, 1.000000000000000000, 0.9510565162951535312, 1.000000000000000000, 0.9510565162951535312, 1.000000000000000000, 0.9510565162951535312, 1.000000000000000000, 0.9510565162951535312, 1.000000000000000000, 0.9510565162951535312, 1.000000000000000000, 0.9510565162951535312, 1.000000000000000000, 0.9510565162951535312, 1.000000000000000000, 0.9510565162951535312, 1.000000000000000000, 0.9510565162951535312, 1.000000000000000000, 0.9510565162951535312, 1.000000000000000000, 0.9510565162951535312, 1.000000000000000000, 0.9510565162951535312, 1.000000000000000000, 0.9510565162951535312, 1.000000000000000000, 0.9510565162951535312, 1.000000000000000000, 0.9510565162951535312, 1.000000000000000000, 0.9510565162951535312, 1.000000000000000000, 0.9510565162951535312, 1.000000000000000000, 0.9510565162951535312, 1.000000000000000000, 0.9510565162951535312, 1.000000000000000000, 0.9510565162951535312, 1.000000000000000000, 0.9510565162951535312, 1.000000000000000000, 0.9510565162951535312, 1.000000000000000000, 0.9510565162951535312, 1.000000000000000000, 0.9510565162951535312, 1.000000000000000000, 0.9510565162951535312, 1.000000000000000000, 0.9510565162951535312, 1.000000000000000000, 0.9510565162951535312, 1.000000000000000000, 0.9510565162951535312, 1.000000000000000000, 0.9510565162951535312, 1.000000000000000000, 0.9510565162951535312, 1.000000000000000000, 0.9510565162951535312, 1.000000000000000000, 0.9510565162951535312, 1.000000000000000000, 0.9510565162951535312, 1.000000000000000000, 0.9510565162951535312, 1.000000000000000000, 0.9510565162951535312, 1.000000000000000000, 0.9510565162951535312, 1.000000000000000000, 0.9510565162951535312, 1.000000000000000000, 0.9510565162951535312, 1.000000000000000000, 0.9510565162951535312, 1.000000000000000000, 0.9510565162951535312, 1.000000000000000000, 0.9510565162951535312, 1.000000000000000000, 0.9510565162951535312, 1.000000000000000000, 0.9510565162951535312, 1.000000000000000000, 0.9510565162951535312, 1.000000000000000000, 0.9510565162951535312, 1.000000000000000000, 0.9510565162951535312, 1.000000000000000000, 0.9510565162951535312, 1.000000000000000000, 0.9510565162951535312, 1.000000000000000000, 0.9510565162951535312, 1.000000000000000000, 0.9510565162951535312, 1.000000000000000000, 0.9510565162951535312, 1.000000000000000000, 0.9510565162951535312, 1.000000000000000000, 0.9510565162951535312, 1.000000000000000000, 0.9510565162951535312, 1.000000000000000000, 0.9510565162951535312, 1.000000000000000000, 0.9510565162951535312, 1.000000000000000000, 0.9510565162951535312, 1.000000000000000000, 0.9510565162951535312, 1.000000000000000000, 0.9510565162951535312, 1.000000000000000000, 0.9510565162951535312, 1.000000000000000000, 0.9510565162951535312, 1.000000000000000000, 0.9510565162951535312, 1.000000000000000000, 0.9510565162951535312, 1.000000000000000000, 0.9510565162951535312, 1.000000000000000000, 0.9510565162951535312, 1.000000000000000000, 0.9510565162951535312, 1.000000000000000000, 0.9510565162951535312, 1.000000000000000000, 0.9510565162951535312, 1.000000000000000000, 0.9510565162951535312, 1.000000000000000000, 0.9510565162951535312, 1.000000000000000000, 0.9510565162951535312, 1.000000000000000000, 0.9510565162951535312, 1.000000000000000000, 0.9510565162951535312, 1.000000000000000000, 0.9510565162951535312, 1.000000000000000000, 0.9510565162951535312, 1.000000000000000000, 0.9510565162951535312, 1.000000000000000000, 0.9510565162951535312, 1.000000000000000000, 0.9510565162951535312, 1.000000000000000000, 0.9510565162951535312, 1.000000000000000000, 0.9510565162951535312, 1.000000000000000000, 0.9510565162951535312, 1.000000000000000000, 0.9510565162951535312, 1.000000000000000000, 0.9510565162951535312, 1.000000000000000000, 0.9510565162951535312, 1.000000000000000000, 0.9510565162951535312, 1.000000000000000000, 0.9510565162951535312, 1.000000000000000000, 0.9510565162951535312, 1.000000000000000000, 0.9510565162951535312, 1.000000000000000000, 0.9510565162951535312, 1.000000000000000000, 0.9510565162951535312, 1.000000000000000000, 0.9510565162951535312, 1.000000000000000000, 0.9510565162951535312, 1.000000000000000000, 0.9510565162951535312, 1.000000000000000000, 0.9510565162951535312, 1.000000000000000000, 0.9510565162951535312, 1.000000000000000000, 0.9510565162951535312, 1.000000000000000000, 0.9510565162951535312, 1.000000000000000000, 0.9510565162951535312, 1.000000000000000000, 0.9510565162951535312, 1.000000000000000000, 0.9510565162951535312, 1.000000000000000000, 0.9510565162951535312, 1.000000000000000000, 0.9703000872435175728, 0.9766452105560685659 ) ) 
 REPRESENTATION_ITEM ( '' )  );
#16361 = EDGE_CURVE ( 'NONE', #16417, #15116, #3202, .T. ) ;
#16362 = CARTESIAN_POINT ( 'NONE',  ( 40.34137639590981905, 24.65937500034139873, 29.30972558990010768 ) ) ;
#16363 = CARTESIAN_POINT ( 'NONE',  ( -15.45084971874737256, 47.38125000068279746, -47.55282581475767500 ) ) ;
#16364 = ORIENTED_EDGE ( 'NONE', *, *, #12618, .T. ) ;
#16365 = EDGE_LOOP ( 'NONE', ( #2472, #7816, #10532, #3298 ) ) ;
#16366 = EDGE_CURVE ( 'NONE', #9091, #6735, #15890, .T. ) ;
#16367 = CARTESIAN_POINT ( 'NONE',  ( -3.219174618344376363E-15, 35.28125000068280315, -52.57311121191334990 ) ) ;
#16368 = AXIS2_PLACEMENT_3D ( 'NONE', #6269, #12666, #1264 ) ;
#16369 = CONICAL_SURFACE ( 'NONE', #4718, 16.50000000000000711, 0.7853981633974447263 ) ;
#16370 = VECTOR ( 'NONE', #8708, 1000.000000000000000 ) ;
#16371 = DIRECTION ( 'NONE',  ( 0.000000000000000000, 0.000000000000000000, -1.000000000000000000 ) ) ;
#16372 = CARTESIAN_POINT ( 'NONE',  ( 14.26268078651494342, 98.74453744460424787, -5.000000000000000000 ) ) ;
#16374 = EDGE_CURVE ( 'NONE', #1181, #6058, #4849, .T. ) ;
#16373 = VECTOR ( 'NONE', #10408, 1000.000000000000000 ) ;
#16375 = VERTEX_POINT ( 'NONE', #7089 ) ;
#16376 = DIRECTION ( 'NONE',  ( -6.938893903907231459E-18, 1.000000000000000000, 5.551115123125782702E-17 ) ) ;
#16377 = CYLINDRICAL_SURFACE ( 'NONE', #5844, 50.00000000000000000 ) ;
#16378 = CARTESIAN_POINT ( 'NONE',  ( -17.01311696148842501, 20.20909521249542706, 101.3333374614808662 ) ) ;
#16379 = FACE_BOUND ( 'NONE', #8231, .T. ) ;
#16380 = CARTESIAN_POINT ( 'NONE',  ( -1.175978673139307859E-14, 45.07596123493892293, -92.05189185291139609 ) ) ;
#16381 = CARTESIAN_POINT ( 'NONE',  ( 4.898587196589413026E-15, 217.0000000000000284, -40.00000000000000000 ) ) ;
#16382 = CARTESIAN_POINT ( 'NONE',  ( 2.464234863135679188, 13.31155363843775064, 101.0000000000000000 ) ) ;
#16383 = EDGE_CURVE ( 'NONE', #6101, #102, #5923, .T. ) ;
#16384 = DIRECTION ( 'NONE',  ( 0.000000000000000000, 1.000000000000000000, 0.000000000000000000 ) ) ;
#16385 = CARTESIAN_POINT ( 'NONE',  ( 15.45084971874737789, 48.38125000068280457, 47.55282581475767500 ) ) ;
#16386 = CARTESIAN_POINT ( 'NONE',  ( 15.45084971874737789, 20.60000000000000142, 47.55282581475767500 ) ) ;
#16387 = VECTOR ( 'NONE', #35, 1000.000000000000227 ) ;
#16388 = CARTESIAN_POINT ( 'NONE',  ( -30.90169943749473802, 24.29999999999999716, 42.53254041760200721 ) ) ;
#16389 = CARTESIAN_POINT ( 'NONE',  ( 9.631387414534489405E-15, 20.35937500034139092, 52.43083105670540789 ) ) ;
#16390 = CARTESIAN_POINT ( 'NONE',  ( -49.99999999999999289, 41.88125000068279746, 16.24598481164533226 ) ) ;
#16391 = AXIS2_PLACEMENT_3D ( 'NONE', #4237, #11710, #4315 ) ;
#16392 = CARTESIAN_POINT ( 'NONE',  ( -49.86468353125000164, 45.85937500034140157, 0.000000000000000000 ) ) ;
#16393 = ORIENTED_EDGE ( 'NONE', *, *, #14306, .F. ) ;
#16394 = DIRECTION ( 'NONE',  ( 0.000000000000000000, -0.7071067811865487940, -0.7071067811865463515 ) ) ;
#16395 = VECTOR ( 'NONE', #3357, 1000.000000000000114 ) ;
#16396 = ORIENTED_EDGE ( 'NONE', *, *, #7214, .T. ) ;
#16397 = DIRECTION ( 'NONE',  ( 0.000000000000000000, 1.000000000000000000, 0.000000000000000000 ) ) ;
#16398 = CARTESIAN_POINT ( 'NONE',  ( -49.86468353124999453, 27.75937500034139660, -16.20201782572375393 ) ) ;
#16399 = VECTOR ( 'NONE', #3151, 1000.000000000000000 ) ;
#16400 = DIRECTION ( 'NONE',  ( -0.000000000000000000, -1.000000000000000000, -0.000000000000000000 ) ) ;
#16401 = CARTESIAN_POINT ( 'NONE',  ( -0.5757193964092639504, 40.00000000000000000, 92.94692077166138233 ) ) ;
#16402 = ADVANCED_FACE ( 'NONE', ( #9827 ), #4514, .F. ) ;
#16403 = CARTESIAN_POINT ( 'NONE',  ( 45.54143403682535052, 25.00000000000000000, -20.30922080093668924 ) ) ;
#16404 = CARTESIAN_POINT ( 'NONE',  ( -2.547328955960238000E-13, 30.28125000068279604, 49.99999999999999289 ) ) ;
#16405 = CARTESIAN_POINT ( 'NONE',  ( 15.40903463028482356, 22.52187500034139589, 47.42413220539093999 ) ) ;
#16406 = CARTESIAN_POINT ( 'NONE',  ( -49.86468353124999453, 23.95937500034138878, 16.20201782572377169 ) ) ;
#16407 = DIRECTION ( 'NONE',  ( 6.938893903907231459E-18, -1.000000000000000000, -5.551115123125782702E-17 ) ) ;
#16408 = EDGE_CURVE ( 'NONE', #10428, #891, #8403, .T. ) ;
#16409 = CARTESIAN_POINT ( 'NONE',  ( 15.40903463028482356, 34.52187500034140299, 47.42413220539093999 ) ) ;
#16410 = CARTESIAN_POINT ( 'NONE',  ( -40.45084971874737789, 29.58125000068279675, -29.38926261462365730 ) ) ;
#16411 = CARTESIAN_POINT ( 'NONE',  ( 15.45084971874737789, 32.60000000000000142, 47.55282581475767500 ) ) ;
#16412 = CARTESIAN_POINT ( 'NONE',  ( 30.81806926056962936, 41.15937500034139873, -42.41743335407647209 ) ) ;
#16413 = CARTESIAN_POINT ( 'NONE',  ( 40.34137639590981905, 28.72187500034139873, 29.30972558990010768 ) ) ;
#16414 = CARTESIAN_POINT ( 'NONE',  ( -30.90169943749473802, 48.30000000000000426, 42.53254041760200721 ) ) ;
#16415 = ORIENTED_EDGE ( 'NONE', *, *, #14653, .T. ) ;
#16416 = CARTESIAN_POINT ( 'NONE',  ( 40.34137639590981195, 39.05937500034140442, -29.30972558990011834 ) ) ;
#16417 = VERTEX_POINT ( 'NONE', #4588 ) ;
#16418 = ORIENTED_EDGE ( 'NONE', *, *, #3535, .T. ) ;
#16419 = CARTESIAN_POINT ( 'NONE',  ( 24.78235906513272724, 286.0218276482402189, -7.282359065131384313 ) ) ;
#16420 = CARTESIAN_POINT ( 'NONE',  ( 50.00000000000000000, 20.78125000068279959, -6.123233995736766085E-15 ) ) ;
#16421 = CARTESIAN_POINT ( 'NONE',  ( -7.919222016226688865, 33.55125428154685352, -50.00000000000003553 ) ) ;
#16422 = CARTESIAN_POINT ( 'NONE',  ( -30.81806926056962226, 22.22187500034139163, 42.41743335407647919 ) ) ;
#16423 = FACE_OUTER_BOUND ( 'NONE', #3468, .T. ) ;
#16424 = CARTESIAN_POINT ( 'NONE',  ( -40.34137639590981195, 42.12187500034139731, 29.30972558990012189 ) ) ;
#16425 = LINE ( 'NONE', #15163, #6309 ) ;
#16426 = EDGE_CURVE ( 'NONE', #5700, #1977, #15747, .T. ) ;
#16427 = CARTESIAN_POINT ( 'NONE',  ( -30.90169943749474868, 45.70000000000000995, -42.53254041760200721 ) ) ;
#16428 = EDGE_CURVE ( 'NONE', #14468, #3644, #10020, .T. ) ;
#16429 = CARTESIAN_POINT ( 'NONE',  ( -49.99999999999999289, 29.68125000068279817, -16.24598481164531449 ) ) ;
#16430 = CARTESIAN_POINT ( 'NONE',  ( 49.86468353124999453, 49.02187500034140299, -16.20201782572376459 ) ) ;
#16431 = CARTESIAN_POINT ( 'NONE',  ( -30.81806926056962226, 34.22187500034139873, 42.41743335407647919 ) ) ;
#16432 = CARTESIAN_POINT ( 'NONE',  ( -20.06446087899944786, 286.3455096218657445, -7.532230439500316344 ) ) ;
#16433 = VECTOR ( 'NONE', #477, 1000.000000000000227 ) ;
#16434 = CARTESIAN_POINT ( 'NONE',  ( -40.45084971874737079, 28.20000000000000284, 29.38926261462367151 ) ) ;
#16435 = ORIENTED_EDGE ( 'NONE', *, *, #8796, .F. ) ;
#16436 = VERTEX_POINT ( 'NONE', #751 ) ;
#16437 = CARTESIAN_POINT ( 'NONE',  ( 50.00000000000000000, 45.00000000000000711, -6.123233995736766085E-15 ) ) ;
#16438 = CARTESIAN_POINT ( 'NONE',  ( -3.749999999999977351, 40.00000000000000711, 6.495190528383290918 ) ) ;
#16439 = DIRECTION ( 'NONE',  ( -6.938893903907231459E-18, 1.000000000000000000, 5.551115123125782702E-17 ) ) ;
#16440 = CARTESIAN_POINT ( 'NONE',  ( 49.86468353125000164, 28.85937500034139802, -6.106662507704105588E-15 ) ) ;
#16441 = DIRECTION ( 'NONE',  ( -0.000000000000000000, 1.000000000000000000, -0.000000000000000000 ) ) ;
#16442 = CARTESIAN_POINT ( 'NONE',  ( 15.40903463028481113, 43.32187500034139305, -47.42413220539094709 ) ) ;
#16443 = AXIS2_PLACEMENT_3D ( 'NONE', #14871, #13624, #6087 ) ;
#16444 =( NAMED_UNIT ( * ) SI_UNIT ( $, .STERADIAN. ) SOLID_ANGLE_UNIT ( ) );
#16445 = CARTESIAN_POINT ( 'NONE',  ( 1.293669679204937499E-13, 39.50000000000000711, -50.00000000000000000 ) ) ;
#16446 = PLANE ( 'NONE',  #3674 ) ;
#16447 = CARTESIAN_POINT ( 'NONE',  ( -49.99999999999999289, 42.09999999999999432, 16.24598481164533226 ) ) ;
#16448 = ORIENTED_EDGE ( 'NONE', *, *, #10794, .F. ) ;
#16449 = CARTESIAN_POINT ( 'NONE',  ( -15.40903463028481646, 27.45937500034139944, -47.42413220539093999 ) ) ;
#16450 = ORIENTED_EDGE ( 'NONE', *, *, #13561, .F. ) ;
#16451 = CARTESIAN_POINT ( 'NONE',  ( 1.087539521958779419E-14, 272.0000000000000000, -87.81953344283027718 ) ) ;
#16452 = EDGE_LOOP ( 'NONE', ( #12807, #15030, #12181, #14611 ) ) ;
#16453 = ORIENTED_EDGE ( 'NONE', *, *, #14582, .F. ) ;
#16454 = VECTOR ( 'NONE', #5807, 1000.000000000000000 ) ;
#16455 = DIRECTION ( 'NONE',  ( -1.000000000000000000, 0.000000000000000000, 0.000000000000000000 ) ) ;
#16456 = LINE ( 'NONE', #15035, #3051 ) ;
#16457 = LINE ( 'NONE', #10224, #12743 ) ;
#16458 = CARTESIAN_POINT ( 'NONE',  ( 0.000000000000000000, 20.00000000000000355, 0.000000000000000000 ) ) ;
#16459 = CARTESIAN_POINT ( 'NONE',  ( 49.99999999999999289, 32.88125000068280457, -16.24598481164532160 ) ) ;
#16460 = CARTESIAN_POINT ( 'NONE',  ( 0.000000000000000000, 22.50000000000000000, 101.0000000000000000 ) ) ;
#16461 = CARTESIAN_POINT ( 'NONE',  ( 8.446640517145639571E-15, 26.28125000068279959, 50.00000000000000000 ) ) ;
#16462 = DIRECTION ( 'NONE',  ( -0.6691306063588671194, 0.7431448254773862505, 0.000000000000000000 ) ) ;
#16463 =( NAMED_UNIT ( * ) SI_UNIT ( $, .STERADIAN. ) SOLID_ANGLE_UNIT ( ) );
#16464 = CARTESIAN_POINT ( 'NONE',  ( 0.000000000000000000, 193.4213562373095385, -50.00000000000000000 ) ) ;
#16465 = DIRECTION ( 'NONE',  ( 0.000000000000000000, 0.000000000000000000, 1.000000000000000000 ) ) ;
#16466 = NEXT_ASSEMBLY_USAGE_OCCURRENCE ( 'NAUO1', ' ', ' ', #6929, #2740, $ ) ;
#16467 = NEXT_ASSEMBLY_USAGE_OCCURRENCE ( 'NAUO2', ' ', ' ', #6929, #11888, $ ) ;
#16468 = NEXT_ASSEMBLY_USAGE_OCCURRENCE ( 'NAUO3', ' ', ' ', #6929, #14821, $ ) ;
#16469 = NEXT_ASSEMBLY_USAGE_OCCURRENCE ( 'NAUO4', ' ', ' ', #6929, #5699, $ ) ;
#16470 = NEXT_ASSEMBLY_USAGE_OCCURRENCE ( 'NAUO5', ' ', ' ', #6929, #295, $ ) ;
#16471 = NEXT_ASSEMBLY_USAGE_OCCURRENCE ( 'NAUO6', ' ', ' ', #6929, #9149, $ ) ;
#16472 = NEXT_ASSEMBLY_USAGE_OCCURRENCE ( 'NAUO7', ' ', ' ', #6929, #4279, $ ) ;
#16473 = NEXT_ASSEMBLY_USAGE_OCCURRENCE ( 'NAUO8', ' ', ' ', #6929, #7215, $ ) ;
#16474 = NEXT_ASSEMBLY_USAGE_OCCURRENCE ( 'NAUO9', ' ', ' ', #6929, #14821, $ ) ;
ENDSEC;
END-ISO-10303-21;
